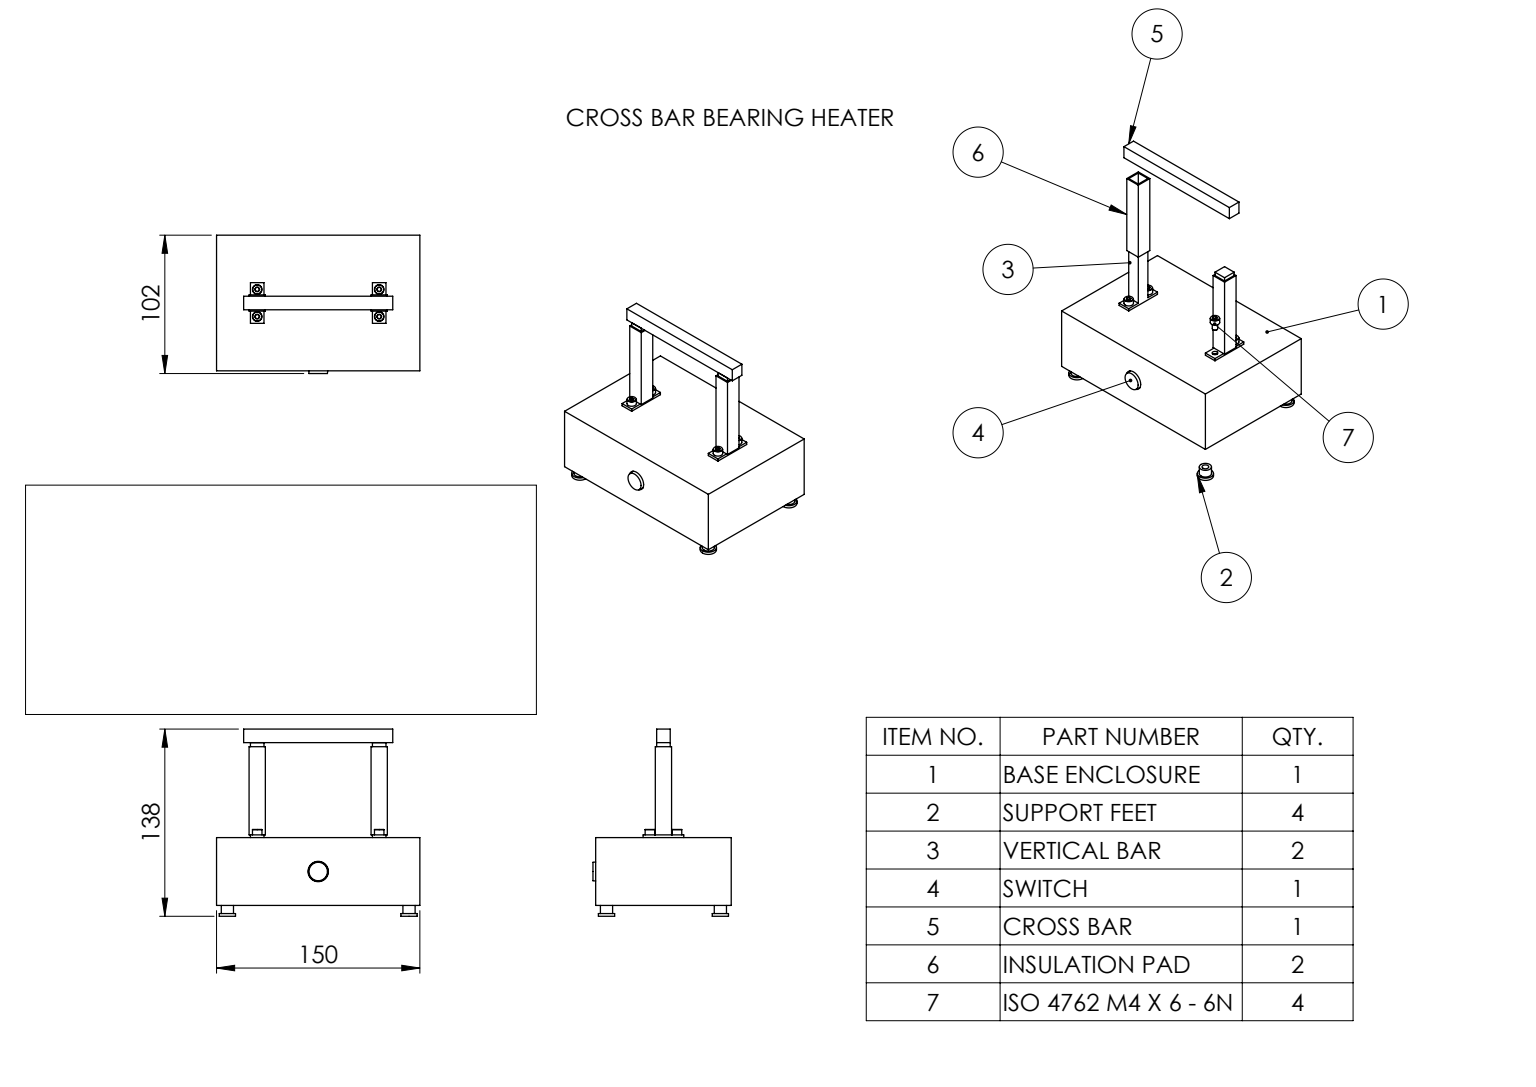
ISO-10303-21;
HEADER;
FILE_DESCRIPTION (('STEP AP214'),
    '1' );
FILE_NAME ('MAS-192',
    '2026-10-24T04:45:50',
    ( '' ),
    ( '' ),
    'SwSTEP 2.0',
    'SolidWorks 2026',
    '' );
FILE_SCHEMA (( 'AUTOMOTIVE_DESIGN' ));
ENDSEC;

DATA;
#1 = ADVANCED_BREP_SHAPE_REPRESENTATION ( '', ( #1992, #3111 ), #2618 ) ;
#2 =( GEOMETRIC_REPRESENTATION_CONTEXT ( 3 ) GLOBAL_UNCERTAINTY_ASSIGNED_CONTEXT ( ( #2528 ) ) GLOBAL_UNIT_ASSIGNED_CONTEXT ( ( #1633, #2133, #1361 ) ) REPRESENTATION_CONTEXT ( 'NONE', 'WORKASPACE' ) );
#3 = DIRECTION ( 'NONE',  ( 0.000000000000000000, -1.000000000000000000, 0.000000000000000000 ) ) ;
#4 = ORIENTED_EDGE ( 'NONE', *, *, #1160, .F. ) ;
#5 = ADVANCED_FACE ( 'NONE', ( #1217, #1180 ), #2474, .T. ) ;
#6 = ORIENTED_EDGE ( 'NONE', *, *, #1808, .T. ) ;
#7 =( GEOMETRIC_REPRESENTATION_CONTEXT ( 3 ) GLOBAL_UNCERTAINTY_ASSIGNED_CONTEXT ( ( #487 ) ) GLOBAL_UNIT_ASSIGNED_CONTEXT ( ( #3000, #1213, #165 ) ) REPRESENTATION_CONTEXT ( 'NONE', 'WORKASPACE' ) );
#8 = DIRECTION ( 'NONE',  ( 0.000000000000000000, 0.000000000000000000, -1.000000000000000000 ) ) ;
#9 = LINE ( 'NONE', #3109, #1942 ) ;
#10 = ORIENTED_EDGE ( 'NONE', *, *, #1397, .T. ) ;
#11 = FACE_OUTER_BOUND ( 'NONE', #1438, .T. ) ;
#12 = FILL_AREA_STYLE_COLOUR ( '', #2947 ) ;
#13 = ORIENTED_EDGE ( 'NONE', *, *, #2082, .F. ) ;
#14 = FACE_OUTER_BOUND ( 'NONE', #3102, .T. ) ;
#15 = FILL_AREA_STYLE_COLOUR ( '', #1949 ) ;
#16 = EDGE_CURVE ( 'NONE', #2394, #756, #2740, .T. ) ;
#17 = DIRECTION ( 'NONE',  ( 0.000000000000000000, 0.000000000000000000, -1.000000000000000000 ) ) ;
#18 = CARTESIAN_POINT ( 'NONE',  ( -49.99999999999999289, 52.00000000000000711, -14.99999999999999645 ) ) ;
#19 = CARTESIAN_POINT ( 'NONE',  ( 66.99999999999997158, -5.000000000000000000, -44.49999999999999289 ) ) ;
#20 = CARTESIAN_POINT ( 'NONE',  ( -40.00000000000000000, 136.9705627484771355, -4.999999999999995559 ) ) ;
#21 = VERTEX_POINT ( 'NONE', #149 ) ;
#22 = VERTEX_POINT ( 'NONE', #1418 ) ;
#23 = CARTESIAN_POINT ( 'NONE',  ( -49.99999999999999289, 136.9705627484771355, -4.999999999999995559 ) ) ;
#24 = EDGE_CURVE ( 'NONE', #3154, #2478, #414, .T. ) ;
#25 = PRODUCT ( 'Support Feet^MAS-192', 'Support Feet^MAS-192', '', ( #945 ) ) ;
#26 = ORIENTED_EDGE ( 'NONE', *, *, #2595, .T. ) ;
#27 = CARTESIAN_POINT ( 'NONE',  ( 2.000000000000000000, -1.773042676681341856, 2.276824562219559311E-15 ) ) ;
#28 = VERTEX_POINT ( 'NONE', #3019 ) ;
#29 = LINE ( 'NONE', #1074, #3100 ) ;
#30 = CARTESIAN_POINT ( 'NONE',  ( -45.00000000000000000, 52.00000000000000711, -7.849999999999996092 ) ) ;
#31 = DIRECTION ( 'NONE',  ( -0.7071067811865355823, 0.000000000000000000, 0.7071067811865595631 ) ) ;
#32 = EDGE_CURVE ( 'NONE', #3203, #1539, #250, .T. ) ;
#33 = LINE ( 'NONE', #1363, #814 ) ;
#34 = ORIENTED_EDGE ( 'NONE', *, *, #997, .F. ) ;
#35 = VERTEX_POINT ( 'NONE', #2248 ) ;
#36 = EDGE_CURVE ( 'NONE', #859, #595, #2266, .T. ) ;
#37 = PLANE ( 'NONE',  #2989 ) ;
#38 = VERTEX_POINT ( 'NONE', #2461 ) ;
#39 = DIRECTION ( 'NONE',  ( -0.000000000000000000, 1.000000000000000000, -0.000000000000000000 ) ) ;
#40 = AXIS2_PLACEMENT_3D ( 'NONE', #1566, #1549, #2083 ) ;
#41 = ORIENTED_EDGE ( 'NONE', *, *, #2652, .T. ) ;
#42 = AXIS2_PLACEMENT_3D ( 'NONE', #131, #167, #900 ) ;
#43 = EDGE_CURVE ( 'NONE', #2320, #2585, #1939, .T. ) ;
#44 = AXIS2_PLACEMENT_3D ( 'NONE', #1214, #1923, #390 ) ;
#45 = LINE ( 'NONE', #1904, #2060 ) ;
#46 =( REPRESENTATION_RELATIONSHIP ('NONE','NONE', #3165, #714 ) REPRESENTATION_RELATIONSHIP_WITH_TRANSFORMATION ( #1813 )SHAPE_REPRESENTATION_RELATIONSHIP( ) );
#47 = AXIS2_PLACEMENT_3D ( 'NONE', #2108, #1339, #2131 ) ;
#48 = FACE_OUTER_BOUND ( 'NONE', #483, .T. ) ;
#49 = AXIS2_PLACEMENT_3D ( 'NONE', #2635, #3135, #2647 ) ;
#50 = CYLINDRICAL_SURFACE ( 'NONE', #2706, 2.000000000000001776 ) ;
#51 = CIRCLE ( 'NONE', #1902, 2.000000000000001776 ) ;
#52 = PRODUCT_DEFINITION_SHAPE ( 'NONE', 'NONE',  #3387 ) ;
#53 = CARTESIAN_POINT ( 'NONE',  ( -51.00000000000000000, 52.00000000000000711, -5.999999999999995559 ) ) ;
#54 = COLOUR_RGB ( '',0.8941176470588234615, 0.8941176470588234615, 0.8941176470588234615 ) ;
#55 = AXIS2_PLACEMENT_3D ( 'NONE', #952, #3052, #3261 ) ;
#56 = ORIENTED_EDGE ( 'NONE', *, *, #736, .T. ) ;
#57 = ORIENTED_EDGE ( 'NONE', *, *, #3226, .F. ) ;
#58 = DIRECTION ( 'NONE',  ( -0.000000000000000000, 1.000000000000000000, -0.000000000000000000 ) ) ;
#59 = VECTOR ( 'NONE', #1910, 1000.000000000000000 ) ;
#60 = EDGE_CURVE ( 'NONE', #1345, #1406, #445, .T. ) ;
#61 = ORIENTED_EDGE ( 'NONE', *, *, #3226, .T. ) ;
#62 = CARTESIAN_POINT ( 'NONE',  ( 75.00000000000000000, 0.000000000000000000, 50.00000000000000000 ) ) ;
#63 = SHAPE_REPRESENTATION_RELATIONSHIP ( 'NONE' , 'NONE' ,  #2804, #1506 ) ;
#64 = EDGE_LOOP ( 'NONE', ( #1744, #977, #3089, #1709 ) ) ;
#65 = CARTESIAN_POINT ( 'NONE',  ( 44.99999999999999289, 50.00000000000000000, -10.00000000000000533 ) ) ;
#66 = PRODUCT_DEFINITION ( 'UNKNOWN', '', #1367, #996 ) ;
#67 = LINE ( 'NONE', #1330, #689 ) ;
#68 = DIRECTION ( 'NONE',  ( -1.000000000000000000, -0.000000000000000000, -0.000000000000000000 ) ) ;
#69 = CARTESIAN_POINT ( 'NONE',  ( -45.00000000000000000, 52.00000000000000711, -9.999999999999994671 ) ) ;
#70 = ORIENTED_EDGE ( 'NONE', *, *, #2599, .T. ) ;
#71 = ORIENTED_EDGE ( 'NONE', *, *, #288, .F. ) ;
#72 = LINE ( 'NONE', #1928, #2609 ) ;
#73 = DIRECTION ( 'NONE',  ( 0.000000000000000000, -0.8660254037844391517, -0.4999999999999991673 ) ) ;
#74 = ORIENTED_EDGE ( 'NONE', *, *, #2863, .T. ) ;
#75 = FACE_OUTER_BOUND ( 'NONE', #670, .T. ) ;
#76 = ADVANCED_FACE ( 'NONE', ( #408 ), #1739, .F. ) ;
#77 = UNCERTAINTY_MEASURE_WITH_UNIT (LENGTH_MEASURE( 1.000000000000000082E-05 ), #1447, 'distance_accuracy_value', 'NONE');
#78 = VERTEX_POINT ( 'NONE', #1445 ) ;
#79 = LINE ( 'NONE', #829, #260 ) ;
#80 = SURFACE_STYLE_USAGE ( .BOTH. , #3231 ) ;
#81 = DIRECTION ( 'NONE',  ( 0.000000000000000000, 0.000000000000000000, -1.000000000000000000 ) ) ;
#82 = LINE ( 'NONE', #1653, #2818 ) ;
#83 = CARTESIAN_POINT ( 'NONE',  ( -51.00000000000000711, 136.9705627484771355, 6.000000000000004441 ) ) ;
#84 = VERTEX_POINT ( 'NONE', #2233 ) ;
#85 = EDGE_LOOP ( 'NONE', ( #3218, #1338, #850, #555, #3293 ) ) ;
#86 = CARTESIAN_POINT ( 'NONE',  ( 4.000000000000000000, 0.000000000000000000, 0.000000000000000000 ) ) ;
#87 = DIRECTION ( 'NONE',  ( 0.000000000000000000, 0.000000000000000000, 1.000000000000000000 ) ) ;
#88 = ORIENTED_EDGE ( 'NONE', *, *, #1626, .T. ) ;
#89 = LINE ( 'NONE', #1159, #2710 ) ;
#90 = EDGE_CURVE ( 'NONE', #872, #1203, #2433, .T. ) ;
#91 = ORIENTED_EDGE ( 'NONE', *, *, #1822, .T. ) ;
#92 = DIRECTION ( 'NONE',  ( 0.000000000000000000, 0.000000000000000000, 1.000000000000000000 ) ) ;
#93 = ADVANCED_FACE ( 'NONE', ( #3005 ), #3282, .F. ) ;
#94 = CIRCLE ( 'NONE', #1191, 2.499999999999995115 ) ;
#95 = CARTESIAN_POINT ( 'NONE',  ( 0.1999999999999987899, 4.286263797015736595E-16, -3.500000000000000000 ) ) ;
#96 = CARTESIAN_POINT ( 'NONE',  ( -74.99999999999998579, 50.00000000000000000, -50.00000000000000000 ) ) ;
#97 = AXIS2_PLACEMENT_3D ( 'NONE', #437, #2770, #128 ) ;
#98 = AXIS2_PLACEMENT_3D ( 'NONE', #3255, #906, #600 ) ;
#99 = DIRECTION ( 'NONE',  ( 0.000000000000000000, -1.000000000000000000, -0.000000000000000000 ) ) ;
#100 = ORIENTED_EDGE ( 'NONE', *, *, #3033, .T. ) ;
#101 = CONICAL_SURFACE ( 'NONE', #2881, 7.250000000000000000, 0.08726646259971666819 ) ;
#102 = EDGE_LOOP ( 'NONE', ( #2901, #2851, #579, #3094 ) ) ;
#103 = FACE_BOUND ( 'NONE', #1561, .T. ) ;
#104 = AXIS2_PLACEMENT_3D ( 'NONE', #3003, #1688, #391 ) ;
#105 = PLANE ( 'NONE',  #1846 ) ;
#106 = EDGE_CURVE ( 'NONE', #871, #1696, #686, .T. ) ;
#107 = SHAPE_REPRESENTATION ( 'cross bar', ( #3111 ), #2618 ) ;
#108 = VERTEX_POINT ( 'NONE', #676 ) ;
#109 =( GEOMETRIC_REPRESENTATION_CONTEXT ( 3 ) GLOBAL_UNCERTAINTY_ASSIGNED_CONTEXT ( ( #1070 ) ) GLOBAL_UNIT_ASSIGNED_CONTEXT ( ( #2231, #2739, #2029 ) ) REPRESENTATION_CONTEXT ( 'NONE', 'WORKASPACE' ) );
#110 = DIRECTION ( 'NONE',  ( -1.000000000000000000, -0.000000000000000000, -0.000000000000000000 ) ) ;
#111 = CARTESIAN_POINT ( 'NONE',  ( 0.000000000000000000, 0.000000000000000000, 0.000000000000000000 ) ) ;
#112 = APPLICATION_CONTEXT ( 'automotive_design' ) ;
#113 = VERTEX_POINT ( 'NONE', #494 ) ;
#114 = AXIS2_PLACEMENT_3D ( 'NONE', #1867, #2907, #1373 ) ;
#115 = CARTESIAN_POINT ( 'NONE',  ( 66.99999999999997158, -5.000000000000000000, -39.50000000000000000 ) ) ;
#116 = DIRECTION ( 'NONE',  ( 4.857225732735056709E-15, 0.000000000000000000, 1.000000000000000000 ) ) ;
#117 = CARTESIAN_POINT ( 'NONE',  ( 9.610000000000013642, 2.449293598294707893E-16, -2.000000000000000888 ) ) ;
#118 = ADVANCED_FACE ( 'NONE', ( #1534 ), #3208, .F. ) ;
#119 = CARTESIAN_POINT ( 'NONE',  ( -74.99999999999998579, 50.00000000000000000, -50.00000000000000000 ) ) ;
#120 = ORIENTED_EDGE ( 'NONE', *, *, #698, .T. ) ;
#121 = VERTEX_POINT ( 'NONE', #1820 ) ;
#122 = FACE_BOUND ( 'NONE', #2327, .T. ) ;
#123 = FACE_OUTER_BOUND ( 'NONE', #1619, .T. ) ;
#124 = ORIENTED_EDGE ( 'NONE', *, *, #674, .T. ) ;
#125 = LINE ( 'NONE', #3241, #2277 ) ;
#126 = PRODUCT_CONTEXT ( 'NONE', #916, 'mechanical' ) ;
#127 = ORIENTED_EDGE ( 'NONE', *, *, #1397, .F. ) ;
#128 = DIRECTION ( 'NONE',  ( 1.000000000000000000, 0.000000000000000000, 0.000000000000000000 ) ) ;
#129 = SURFACE_STYLE_FILL_AREA ( #3049 ) ;
#130 = LINE ( 'NONE', #2502, #3267 ) ;
#131 = CARTESIAN_POINT ( 'NONE',  ( 10.00000000000000000, 1.610000000000000098, 0.000000000000000000 ) ) ;
#132 = CARTESIAN_POINT ( 'NONE',  ( -66.99999999999997158, 0.000000000000000000, -41.99999999999999289 ) ) ;
#133 = EDGE_CURVE ( 'NONE', #3190, #3154, #2535, .T. ) ;
#134 = CARTESIAN_POINT ( 'NONE',  ( 0.000000000000000000, 25.00000000000000000, 50.00000000000000000 ) ) ;
#135 = FACE_OUTER_BOUND ( 'NONE', #3028, .T. ) ;
#136 = CARTESIAN_POINT ( 'NONE',  ( 0.000000000000000000, 117.0000000000000000, 0.000000000000000000 ) ) ;
#137 = EDGE_CURVE ( 'NONE', #1848, #2577, #1400, .T. ) ;
#138 = ORIENTED_EDGE ( 'NONE', *, *, #2911, .T. ) ;
#139 = CARTESIAN_POINT ( 'NONE',  ( 10.00000000000000178, 0.000000000000000000, 0.000000000000000000 ) ) ;
#140 = UNCERTAINTY_MEASURE_WITH_UNIT (LENGTH_MEASURE( 1.000000000000000082E-05 ), #3331, 'distance_accuracy_value', 'NONE');
#141 = CARTESIAN_POINT ( 'NONE',  ( 0.000000000000000000, 0.000000000000000000, 0.000000000000000000 ) ) ;
#142 = ORIENTED_EDGE ( 'NONE', *, *, #43, .F. ) ;
#143 = CARTESIAN_POINT ( 'NONE',  ( -49.99999999999998579, 50.00000000000000000, 15.00000000000000888 ) ) ;
#144 = EDGE_CURVE ( 'NONE', #1979, #3353, #770, .T. ) ;
#145 = DIRECTION ( 'NONE',  ( -0.000000000000000000, 1.000000000000000000, -0.000000000000000000 ) ) ;
#146 = DIRECTION ( 'NONE',  ( 0.000000000000000000, -1.000000000000000000, 0.000000000000000000 ) ) ;
#147 = CIRCLE ( 'NONE', #1023, 2.000000000000000888 ) ;
#148 = DIRECTION ( 'NONE',  ( -0.000000000000000000, 1.000000000000000000, -0.000000000000000000 ) ) ;
#149 = CARTESIAN_POINT ( 'NONE',  ( 4.000000000000001776, 0.000000000000000000, -2.200000000000001066 ) ) ;
#150 = AXIS2_PLACEMENT_3D ( 'NONE', #1095, #3156, #1856 ) ;
#151 = DIRECTION ( 'NONE',  ( 1.000000000000000000, 0.000000000000000000, 0.000000000000000000 ) ) ;
#152 = VECTOR ( 'NONE', #2701, 1000.000000000000000 ) ;
#153 = MECHANICAL_DESIGN_GEOMETRIC_PRESENTATION_REPRESENTATION (  '', ( #3211 ), #1787 ) ;
#154 = VECTOR ( 'NONE', #3115, 1000.000000000000114 ) ;
#155 = ORIENTED_EDGE ( 'NONE', *, *, #2097, .T. ) ;
#156 = DIRECTION ( 'NONE',  ( 1.000000000000000000, 0.000000000000000000, -0.000000000000000000 ) ) ;
#157 = VECTOR ( 'NONE', #2892, 1000.000000000000227 ) ;
#158 = CIRCLE ( 'NONE', #2772, 2.499999999999995115 ) ;
#159 = EDGE_CURVE ( 'NONE', #28, #1965, #1834, .T. ) ;
#160 = DIRECTION ( 'NONE',  ( 0.000000000000000000, 0.000000000000000000, -1.000000000000000000 ) ) ;
#161 = MECHANICAL_DESIGN_GEOMETRIC_PRESENTATION_REPRESENTATION (  '', ( #2503 ), #1797 ) ;
#162 = EDGE_LOOP ( 'NONE', ( #2034, #1285, #2151, #1503 ) ) ;
#163 = DIRECTION ( 'NONE',  ( -1.000000000000000000, -0.000000000000000000, -0.000000000000000000 ) ) ;
#164 = VECTOR ( 'NONE', #3281, 1000.000000000000000 ) ;
#165 =( NAMED_UNIT ( * ) SI_UNIT ( $, .STERADIAN. ) SOLID_ANGLE_UNIT ( ) );
#166 = FACE_OUTER_BOUND ( 'NONE', #3168, .T. ) ;
#167 = DIRECTION ( 'NONE',  ( 1.000000000000000000, 0.000000000000000000, 0.000000000000000000 ) ) ;
#168 = ADVANCED_FACE ( 'NONE', ( #219 ), #472, .F. ) ;
#169 = AXIS2_PLACEMENT_3D ( 'NONE', #1933, #1186, #2975 ) ;
#170 = CARTESIAN_POINT ( 'NONE',  ( -75.00000000000000000, 50.00000000000000000, 50.00000000000000000 ) ) ;
#171 = PLANE ( 'NONE',  #1465 ) ;
#172 = DIRECTION ( 'NONE',  ( 0.000000000000000000, 0.000000000000000000, -1.000000000000000000 ) ) ;
#173 = EDGE_LOOP ( 'NONE', ( #2677, #3008, #1781, #962 ) ) ;
#174 = CARTESIAN_POINT ( 'NONE',  ( -44.99999999999999289, 52.00000000000000711, 10.00000000000000533 ) ) ;
#175 = APPLICATION_PROTOCOL_DEFINITION ( 'draft international standard', 'automotive_design', 1998, #2030 ) ;
#176 = ORIENTED_EDGE ( 'NONE', *, *, #433, .T. ) ;
#177 = ADVANCED_FACE ( 'NONE', ( #782 ), #2573, .F. ) ;
#178 = CARTESIAN_POINT ( 'NONE',  ( 44.99999999999999289, 50.00000000000000000, -12.00000000000000711 ) ) ;
#179 = SHAPE_REPRESENTATION_RELATIONSHIP ( 'NONE' , 'NONE' ,  #1050, #930 ) ;
#180 = ORIENTED_EDGE ( 'NONE', *, *, #1149, .T. ) ;
#181 = EDGE_CURVE ( 'NONE', #2222, #1240, #233, .T. ) ;
#182 = DIRECTION ( 'NONE',  ( 0.000000000000000000, 0.4999999999999989453, -0.8660254037844391517 ) ) ;
#183 = DIRECTION ( 'NONE',  ( -0.000000000000000000, 1.000000000000000000, -0.000000000000000000 ) ) ;
#184 = LINE ( 'NONE', #1230, #2344 ) ;
#185 = DIRECTION ( 'NONE',  ( -0.000000000000000000, 1.000000000000000000, 0.000000000000000000 ) ) ;
#186 = CARTESIAN_POINT ( 'NONE',  ( -66.99999999999997158, -5.000000000000000000, -41.99999999999999289 ) ) ;
#187 = ADVANCED_FACE ( 'NONE', ( #2861 ), #2830, .F. ) ;
#188 = ORIENTED_EDGE ( 'NONE', *, *, #783, .T. ) ;
#189 = DIRECTION ( 'NONE',  ( 0.000000000000000000, 0.000000000000000000, 1.000000000000000000 ) ) ;
#190 = VERTEX_POINT ( 'NONE', #1045 ) ;
#191 = CARTESIAN_POINT ( 'NONE',  ( -45.00000000000000000, 43.79827876194489278, -9.999999999999994671 ) ) ;
#192 = ORIENTED_EDGE ( 'NONE', *, *, #815, .F. ) ;
#193 = DIRECTION ( 'NONE',  ( -4.857225732735056709E-15, 0.000000000000000000, -1.000000000000000000 ) ) ;
#194 = CARTESIAN_POINT ( 'NONE',  ( -49.99999999999999289, 52.00000000000000711, -4.999999999999995559 ) ) ;
#195 = EDGE_CURVE ( 'NONE', #2855, #2405, #2542, .T. ) ;
#196 = CARTESIAN_POINT ( 'NONE',  ( -51.00000000000000000, 136.9705627484771355, -5.999999999999995559 ) ) ;
#197 = DIRECTION ( 'NONE',  ( -0.000000000000000000, 1.000000000000000000, -0.000000000000000000 ) ) ;
#198 = CARTESIAN_POINT ( 'NONE',  ( -50.00000000000000000, 120.0000000000000142, 5.000000000000004441 ) ) ;
#199 = DIRECTION ( 'NONE',  ( 0.000000000000000000, 0.000000000000000000, -1.000000000000000000 ) ) ;
#200 = EDGE_LOOP ( 'NONE', ( #2592, #100, #1336, #1799 ) ) ;
#201 = VECTOR ( 'NONE', #2928, 1000.000000000000000 ) ;
#202 = CIRCLE ( 'NONE', #44, 6.812556682370379590 ) ;
#203 = ORIENTED_EDGE ( 'NONE', *, *, #133, .F. ) ;
#204 = LINE ( 'NONE', #550, #154 ) ;
#205 = EDGE_CURVE ( 'NONE', #575, #3353, #2981, .T. ) ;
#206 = AXIS2_PLACEMENT_3D ( 'NONE', #944, #2253, #978 ) ;
#207 = ITEM_DEFINED_TRANSFORMATION ( 'NONE', 'NONE', #710,  #3111 ) ;
#208 = ORIENTED_EDGE ( 'NONE', *, *, #1510, .T. ) ;
#209 = CIRCLE ( 'NONE', #2120, 2.499999999999995115 ) ;
#210 = CIRCLE ( 'NONE', #2393, 0.2000000000000000944 ) ;
#211 = DIRECTION ( 'NONE',  ( 0.000000000000000000, -1.000000000000000000, 0.000000000000000000 ) ) ;
#212 = AXIS2_PLACEMENT_3D ( 'NONE', #1617, #2642, #885 ) ;
#213 = VECTOR ( 'NONE', #1718, 1000.000000000000000 ) ;
#214 = ORIENTED_EDGE ( 'NONE', *, *, #2529, .F. ) ;
#215 = CARTESIAN_POINT ( 'NONE',  ( -40.00000000000000000, 52.00000000000000711, -4.999999999999995559 ) ) ;
#216 =( NAMED_UNIT ( * ) PLANE_ANGLE_UNIT ( ) SI_UNIT ( $, .RADIAN. ) );
#217 = CARTESIAN_POINT ( 'NONE',  ( -45.00000000000000000, 50.00000000000000000, -9.999999999999994671 ) ) ;
#218 = PRESENTATION_LAYER_ASSIGNMENT (  '', '', ( #384 ) ) ;
#219 = FACE_OUTER_BOUND ( 'NONE', #3264, .T. ) ;
#220 = EDGE_CURVE ( 'NONE', #2968, #788, #147, .T. ) ;
#221 = DIRECTION ( 'NONE',  ( 0.000000000000000000, 0.4999999999999989453, -0.8660254037844391517 ) ) ;
#222 = DIRECTION ( 'NONE',  ( -0.000000000000000000, 1.000000000000000000, -0.000000000000000000 ) ) ;
#223 = VERTEX_POINT ( 'NONE', #2047 ) ;
#224 = ORIENTED_EDGE ( 'NONE', *, *, #1328, .F. ) ;
#225 = FACE_OUTER_BOUND ( 'NONE', #834, .T. ) ;
#226 = ORIENTED_EDGE ( 'NONE', *, *, #721, .T. ) ;
#227 = CARTESIAN_POINT ( 'NONE',  ( 7.500000000000000000, 25.00000000000000000, 50.00000000000000000 ) ) ;
#228 =( NAMED_UNIT ( * ) SI_UNIT ( $, .STERADIAN. ) SOLID_ANGLE_UNIT ( ) );
#229 = VERTEX_POINT ( 'NONE', #2063 ) ;
#230 =( NAMED_UNIT ( * ) SI_UNIT ( $, .STERADIAN. ) SOLID_ANGLE_UNIT ( ) );
#231 = CARTESIAN_POINT ( 'NONE',  ( 2.000000000000000000, 1.773042676681340524, -2.059984127722458425E-15 ) ) ;
#232 = CARTESIAN_POINT ( 'NONE',  ( 45.00000000000000000, 50.00000000000000000, 9.999999999999994671 ) ) ;
#233 = LINE ( 'NONE', #18, #635 ) ;
#234 = CARTESIAN_POINT ( 'NONE',  ( 66.99999999999997158, 0.000000000000000000, -41.99999999999999289 ) ) ;
#235 = PRODUCT ( 'vertical bar^MAS-192', 'vertical bar^MAS-192', '', ( #1405 ) ) ;
#236 = ADVANCED_FACE ( 'NONE', ( #2285 ), #2096, .F. ) ;
#237 = EDGE_LOOP ( 'NONE', ( #1273, #3223, #1162, #2040 ) ) ;
#238 = ORIENTED_EDGE ( 'NONE', *, *, #3134, .T. ) ;
#239 = DIRECTION ( 'NONE',  ( 1.000000000000000000, 0.000000000000000000, 0.000000000000000000 ) ) ;
#240 = PRODUCT_DEFINITION_CONTEXT ( 'detailed design', #1502, 'design' ) ;
#241 = EDGE_CURVE ( 'NONE', #1406, #684, #9, .T. ) ;
#242 = CONTEXT_DEPENDENT_SHAPE_REPRESENTATION ( #1463, #296 ) ;
#243 = EDGE_LOOP ( 'NONE', ( #2805, #1759, #1997, #2614 ) ) ;
#244 = DIRECTION ( 'NONE',  ( 0.000000000000000000, 0.000000000000000000, 1.000000000000000000 ) ) ;
#245 = ORIENTED_EDGE ( 'NONE', *, *, #2920, .T. ) ;
#246 = CARTESIAN_POINT ( 'NONE',  ( -44.99999999999999289, 45.00000000000000711, 12.00000000000000711 ) ) ;
#247 = SURFACE_SIDE_STYLE ('',( #3334 ) ) ;
#248 = EDGE_CURVE ( 'NONE', #1538, #561, #458, .T. ) ;
#249 = CARTESIAN_POINT ( 'NONE',  ( 0.000000000000000000, 0.8865213383406715941, 1.535499999999999199 ) ) ;
#250 = CIRCLE ( 'NONE', #2594, 2.000000000000001776 ) ;
#251 = CARTESIAN_POINT ( 'NONE',  ( -66.99999999999997158, -6.000000000000000000, 41.99999999999999289 ) ) ;
#252 = DIRECTION ( 'NONE',  ( 0.000000000000000000, 0.000000000000000000, 1.000000000000000000 ) ) ;
#253 = CARTESIAN_POINT ( 'NONE',  ( -40.00000000000000000, 52.00000000000000711, 5.000000000000004441 ) ) ;
#254 = ORIENTED_EDGE ( 'NONE', *, *, #2827, .T. ) ;
#255 = ORIENTED_EDGE ( 'NONE', *, *, #1651, .T. ) ;
#256 = PLANE ( 'NONE',  #3270 ) ;
#257 = CIRCLE ( 'NONE', #2169, 0.2000000000000000944 ) ;
#258 = EDGE_LOOP ( 'NONE', ( #2050, #2619 ) ) ;
#259 = EDGE_CURVE ( 'NONE', #2577, #1848, #1348, .T. ) ;
#260 = VECTOR ( 'NONE', #1128, 1000.000000000000000 ) ;
#261 = CARTESIAN_POINT ( 'NONE',  ( -66.99999999999997158, -8.000000000000000000, 41.99999999999999289 ) ) ;
#262 = CIRCLE ( 'NONE', #1350, 1.610000000000000098 ) ;
#263 = AXIS2_PLACEMENT_3D ( 'NONE', #2360, #1555, #2633 ) ;
#264 = ORIENTED_EDGE ( 'NONE', *, *, #1320, .T. ) ;
#265 = DIRECTION ( 'NONE',  ( 0.000000000000000000, 0.000000000000000000, -1.000000000000000000 ) ) ;
#266 = PRODUCT_DEFINITION_SHAPE ( 'NONE', 'NONE',  #2270 ) ;
#267 = DIRECTION ( 'NONE',  ( -0.000000000000000000, -1.000000000000000000, -0.000000000000000000 ) ) ;
#268 = AXIS2_PLACEMENT_3D ( 'NONE', #2067, #1047, #3088 ) ;
#269 = VECTOR ( 'NONE', #221, 1000.000000000000227 ) ;
#270 = CYLINDRICAL_SURFACE ( 'NONE', #435, 2.000000000000001776 ) ;
#271 = VECTOR ( 'NONE', #3335, 1000.000000000000000 ) ;
#272 = DIRECTION ( 'NONE',  ( 1.000000000000000000, 0.000000000000000000, 0.000000000000000000 ) ) ;
#273 = PRODUCT_DEFINITION ( 'UNKNOWN', '', #2401, #2052 ) ;
#274 = CARTESIAN_POINT ( 'NONE',  ( 2.000000000000000000, -1.773042676681341856, 2.276824562219559311E-15 ) ) ;
#275 = PRESENTATION_LAYER_ASSIGNMENT (  '', '', ( #1313 ) ) ;
#276 = CARTESIAN_POINT ( 'NONE',  ( 7.250000000000000000, 25.00000000000000000, 47.00000000000000000 ) ) ;
#277 = VERTEX_POINT ( 'NONE', #2558 ) ;
#278 = ORIENTED_EDGE ( 'NONE', *, *, #1945, .T. ) ;
#279 = AXIS2_PLACEMENT_3D ( 'NONE', #1513, #2605, #2846 ) ;
#280 = DIRECTION ( 'NONE',  ( 0.000000000000000000, 0.000000000000000000, -1.000000000000000000 ) ) ;
#281 = ORIENTED_EDGE ( 'NONE', *, *, #304, .T. ) ;
#282 = DIRECTION ( 'NONE',  ( -1.000000000000000000, 0.000000000000000000, 0.000000000000000000 ) ) ;
#283 = EDGE_CURVE ( 'NONE', #2585, #480, #1268, .T. ) ;
#284 =( NAMED_UNIT ( * ) SI_UNIT ( $, .STERADIAN. ) SOLID_ANGLE_UNIT ( ) );
#285 = ORIENTED_EDGE ( 'NONE', *, *, #1596, .F. ) ;
#286 = CARTESIAN_POINT ( 'NONE',  ( 75.00000000000000000, 50.00000000000000000, 50.00000000000000000 ) ) ;
#287 = APPLICATION_CONTEXT ( 'automotive_design' ) ;
#288 = EDGE_CURVE ( 'NONE', #788, #2968, #3262, .T. ) ;
#289 = FACE_OUTER_BOUND ( 'NONE', #2539, .T. ) ;
#290 = DIRECTION ( 'NONE',  ( -0.000000000000000000, 1.000000000000000000, -0.000000000000000000 ) ) ;
#291 = CYLINDRICAL_SURFACE ( 'NONE', #701, 4.500000000000010658 ) ;
#292 = ORIENTED_EDGE ( 'NONE', *, *, #3182, .F. ) ;
#293 = ORIENTED_EDGE ( 'NONE', *, *, #658, .F. ) ;
#294 = CYLINDRICAL_SURFACE ( 'NONE', #263, 2.000000000000001776 ) ;
#295 = EDGE_CURVE ( 'NONE', #1203, #575, #3205, .T. ) ;
#296 = PRODUCT_DEFINITION_SHAPE ( 'NONE', 'NONE',  #3383 ) ;
#297 = ORIENTED_EDGE ( 'NONE', *, *, #467, .F. ) ;
#298 = CYLINDRICAL_SURFACE ( 'NONE', #3325, 2.499999999999995115 ) ;
#299 = ORIENTED_EDGE ( 'NONE', *, *, #1600, .T. ) ;
#300 = DIRECTION ( 'NONE',  ( -0.000000000000000000, 1.000000000000000000, -0.000000000000000000 ) ) ;
#301 = SURFACE_STYLE_USAGE ( .BOTH. , #1377 ) ;
#302 = FACE_BOUND ( 'NONE', #1880, .T. ) ;
#303 = PLANE ( 'NONE',  #477 ) ;
#304 = EDGE_CURVE ( 'NONE', #820, #28, #1614, .T. ) ;
#305 = LINE ( 'NONE', #901, #2667 ) ;
#306 = ORIENTED_EDGE ( 'NONE', *, *, #1644, .T. ) ;
#307 = ORIENTED_EDGE ( 'NONE', *, *, #2205, .T. ) ;
#308 = LINE ( 'NONE', #1347, #2939 ) ;
#309 = VERTEX_POINT ( 'NONE', #1378 ) ;
#310 = EDGE_CURVE ( 'NONE', #2398, #468, #2110, .T. ) ;
#311 = FACE_OUTER_BOUND ( 'NONE', #2869, .T. ) ;
#312 = CARTESIAN_POINT ( 'NONE',  ( 0.000000000000000000, 0.000000000000000000, 0.000000000000000000 ) ) ;
#313 = ORIENTED_EDGE ( 'NONE', *, *, #934, .T. ) ;
#314 = AXIS2_PLACEMENT_3D ( 'NONE', #1704, #183, #1430 ) ;
#315 = ADVANCED_BREP_SHAPE_REPRESENTATION ( '', ( #2820, #3111 ), #7 ) ;
#316 = LINE ( 'NONE', #2146, #2603 ) ;
#317 = CIRCLE ( 'NONE', #47, 7.250000000000000000 ) ;
#318 = CIRCLE ( 'NONE', #2498, 2.149999999999999023 ) ;
#319 = DIRECTION ( 'NONE',  ( 0.000000000000000000, -1.000000000000000000, 0.000000000000000000 ) ) ;
#320 = AXIS2_PLACEMENT_3D ( 'NONE', #3066, #1000, #486 ) ;
#321 = LINE ( 'NONE', #1331, #636 ) ;
#322 = AXIS2_PLACEMENT_3D ( 'NONE', #1317, #3110, #3142 ) ;
#323 = CARTESIAN_POINT ( 'NONE',  ( 45.00000000000000000, 45.00000000000000711, 7.999999999999992895 ) ) ;
#324 = VECTOR ( 'NONE', #1168, 999.9999999999998863 ) ;
#325 = EDGE_CURVE ( 'NONE', #1539, #3203, #1947, .T. ) ;
#326 = ORIENTED_EDGE ( 'NONE', *, *, #789, .T. ) ;
#327 = EDGE_LOOP ( 'NONE', ( #1272, #3114, #2142, #1931 ) ) ;
#328 = FACE_OUTER_BOUND ( 'NONE', #327, .T. ) ;
#329 = MECHANICAL_DESIGN_GEOMETRIC_PRESENTATION_REPRESENTATION (  '', ( #1259 ), #109 ) ;
#330 = CYLINDRICAL_SURFACE ( 'NONE', #1898, 2.000000000000001776 ) ;
#331 = VERTEX_POINT ( 'NONE', #2651 ) ;
#332 = LINE ( 'NONE', #2410, #1914 ) ;
#333 =( LENGTH_UNIT ( ) NAMED_UNIT ( * ) SI_UNIT ( .MILLI., .METRE. ) );
#334 = SHAPE_REPRESENTATION_RELATIONSHIP ( 'NONE' , 'NONE' ,  #1286, #3149 ) ;
#335 = ORIENTED_EDGE ( 'NONE', *, *, #1134, .T. ) ;
#336 = DIRECTION ( 'NONE',  ( 6.938893903907228378E-16, 0.000000000000000000, 1.000000000000000000 ) ) ;
#337 = FACE_OUTER_BOUND ( 'NONE', #2632, .T. ) ;
#338 = CARTESIAN_POINT ( 'NONE',  ( 2.000000000000000000, 0.8865213383406680414, -1.535500000000000975 ) ) ;
#339 = LINE ( 'NONE', #83, #1798 ) ;
#340 = ORIENTED_EDGE ( 'NONE', *, *, #1808, .F. ) ;
#341 = ORIENTED_EDGE ( 'NONE', *, *, #1510, .F. ) ;
#342 = DIRECTION ( 'NONE',  ( 1.000000000000000000, 0.000000000000000000, 0.000000000000000000 ) ) ;
#343 = EDGE_CURVE ( 'NONE', #2100, #2365, #797, .T. ) ;
#344 = CARTESIAN_POINT ( 'NONE',  ( -49.99999999999999289, 52.00000000000000711, -14.99999999999999645 ) ) ;
#345 = ORIENTED_EDGE ( 'NONE', *, *, #1998, .T. ) ;
#346 = DIRECTION ( 'NONE',  ( -1.000000000000000000, -0.000000000000000000, -0.000000000000000000 ) ) ;
#347 = VERTEX_POINT ( 'NONE', #3209 ) ;
#348 = CARTESIAN_POINT ( 'NONE',  ( -66.99999999999997158, 0.000000000000000000, 46.50000000000000711 ) ) ;
#349 = SURFACE_STYLE_FILL_AREA ( #2686 ) ;
#350 = DIRECTION ( 'NONE',  ( -0.000000000000000000, 1.000000000000000000, -0.000000000000000000 ) ) ;
#351 = DIRECTION ( 'NONE',  ( 0.000000000000000000, 0.000000000000000000, -1.000000000000000000 ) ) ;
#352 = EDGE_CURVE ( 'NONE', #2026, #820, #262, .T. ) ;
#353 = FACE_OUTER_BOUND ( 'NONE', #793, .T. ) ;
#354 = ORIENTED_EDGE ( 'NONE', *, *, #2172, .F. ) ;
#355 = EDGE_LOOP ( 'NONE', ( #2017, #2646, #2374, #1630 ) ) ;
#356 = LINE ( 'NONE', #823, #1685 ) ;
#357 = FACE_BOUND ( 'NONE', #1452, .T. ) ;
#358 = ORIENTED_EDGE ( 'NONE', *, *, #750, .T. ) ;
#359 = CARTESIAN_POINT ( 'NONE',  ( -44.99999999999999289, 50.00000000000000000, 10.00000000000000533 ) ) ;
#360 =( NAMED_UNIT ( * ) PLANE_ANGLE_UNIT ( ) SI_UNIT ( $, .RADIAN. ) );
#361 = VERTEX_POINT ( 'NONE', #3180 ) ;
#362 = ADVANCED_FACE ( 'NONE', ( #830 ), #478, .F. ) ;
#363 = LINE ( 'NONE', #1728, #583 ) ;
#364 =( LENGTH_UNIT ( ) NAMED_UNIT ( * ) SI_UNIT ( .MILLI., .METRE. ) );
#365 = MECHANICAL_DESIGN_GEOMETRIC_PRESENTATION_REPRESENTATION (  '', ( #2220 ), #1676 ) ;
#366 = AXIS2_PLACEMENT_3D ( 'NONE', #1458, #3294, #1985 ) ;
#367 = FACE_OUTER_BOUND ( 'NONE', #3150, .T. ) ;
#368 = DIRECTION ( 'NONE',  ( 0.000000000000000000, 0.000000000000000000, 1.000000000000000000 ) ) ;
#369 = VECTOR ( 'NONE', #2367, 1000.000000000000000 ) ;
#370 = CIRCLE ( 'NONE', #482, 4.500000000000010658 ) ;
#371 = DIRECTION ( 'NONE',  ( -1.000000000000000000, -0.000000000000000000, -0.000000000000000000 ) ) ;
#372 = ORIENTED_EDGE ( 'NONE', *, *, #3079, .F. ) ;
#373 = AXIS2_PLACEMENT_3D ( 'NONE', #3007, #3300, #957 ) ;
#374 = EDGE_CURVE ( 'NONE', #2968, #21, #257, .T. ) ;
#375 = CIRCLE ( 'NONE', #1306, 2.499999999999995115 ) ;
#376 = ORIENTED_EDGE ( 'NONE', *, *, #1556, .T. ) ;
#377 = FACE_BOUND ( 'NONE', #2636, .T. ) ;
#378 = CIRCLE ( 'NONE', #212, 3.500000000000000000 ) ;
#379 = AXIS2_PLACEMENT_3D ( 'NONE', #915, #146, #2518 ) ;
#380 = DIRECTION ( 'NONE',  ( 0.000000000000000000, -0.000000000000000000, 1.000000000000000000 ) ) ;
#381 = ORIENTED_EDGE ( 'NONE', *, *, #248, .F. ) ;
#382 = CIRCLE ( 'NONE', #279, 2.499999999999995115 ) ;
#383 = CARTESIAN_POINT ( 'NONE',  ( 2.000000000000000000, 0.000000000000000000, 0.000000000000000000 ) ) ;
#384 = STYLED_ITEM ( 'NONE', ( #3081 ), #1 ) ;
#385 = DIRECTION ( 'NONE',  ( 0.000000000000000000, 0.000000000000000000, -1.000000000000000000 ) ) ;
#386 = ORIENTED_EDGE ( 'NONE', *, *, #1705, .F. ) ;
#387 = AXIS2_PLACEMENT_3D ( 'NONE', #2488, #151, #2249 ) ;
#388 = DIRECTION ( 'NONE',  ( 0.000000000000000000, 0.000000000000000000, -1.000000000000000000 ) ) ;
#389 = ADVANCED_FACE ( 'NONE', ( #337 ), #751, .T. ) ;
#390 = DIRECTION ( 'NONE',  ( 1.000000000000000000, 0.000000000000000000, 0.000000000000000000 ) ) ;
#391 = DIRECTION ( 'NONE',  ( 0.000000000000000000, 1.224646799147353207E-16, 1.000000000000000000 ) ) ;
#392 = EDGE_CURVE ( 'NONE', #2543, #2273, #1858, .T. ) ;
#393 = FACE_OUTER_BOUND ( 'NONE', #821, .T. ) ;
#394 = DIRECTION ( 'NONE',  ( 0.000000000000000000, 0.000000000000000000, 1.000000000000000000 ) ) ;
#395 = CARTESIAN_POINT ( 'NONE',  ( 2.000000000000000000, -0.8865213383406694847, 1.535500000000001419 ) ) ;
#396 = APPLICATION_CONTEXT ( 'automotive_design' ) ;
#397 = DIRECTION ( 'NONE',  ( 0.000000000000000000, 0.4999999999999991118, -0.8660254037844390407 ) ) ;
#398 = ORIENTED_EDGE ( 'NONE', *, *, #2812, .T. ) ;
#399 = DIRECTION ( 'NONE',  ( -0.000000000000000000, 1.000000000000000000, -0.000000000000000000 ) ) ;
#400 = ADVANCED_FACE ( 'NONE', ( #302, #1340 ), #2369, .F. ) ;
#401 = PRODUCT_CONTEXT ( 'NONE', #1167, 'mechanical' ) ;
#402 = ORIENTED_EDGE ( 'NONE', *, *, #3206, .F. ) ;
#403 = CARTESIAN_POINT ( 'NONE',  ( 66.99999999999997158, -5.000000000000000000, -41.99999999999999289 ) ) ;
#404 = FILL_AREA_STYLE_COLOUR ( '', #874 ) ;
#405 = CARTESIAN_POINT ( 'NONE',  ( -66.99999999999997158, -8.000000000000000000, 39.49999999999998579 ) ) ;
#406 = CARTESIAN_POINT ( 'NONE',  ( -51.00000000000000000, 136.9705627484771355, -4.999999999999996447 ) ) ;
#407 = CARTESIAN_POINT ( 'NONE',  ( -45.00000000000000000, 50.00000000000000000, -7.999999999999992895 ) ) ;
#408 = FACE_OUTER_BOUND ( 'NONE', #1187, .T. ) ;
#409 = EDGE_CURVE ( 'NONE', #2129, #108, #67, .T. ) ;
#410 = DIRECTION ( 'NONE',  ( -1.000000000000000000, -0.000000000000000000, 2.365532012695647326E-17 ) ) ;
#411 = ORIENTED_EDGE ( 'NONE', *, *, #2806, .T. ) ;
#412 = PLANE ( 'NONE',  #1407 ) ;
#413 = DIRECTION ( 'NONE',  ( -1.000000000000000000, 0.000000000000000000, 0.000000000000000000 ) ) ;
#414 = CIRCLE ( 'NONE', #849, 7.500000000000000000 ) ;
#415 = ORIENTED_EDGE ( 'NONE', *, *, #2685, .T. ) ;
#416 = EDGE_CURVE ( 'NONE', #2252, #436, #1895, .T. ) ;
#417 = CARTESIAN_POINT ( 'NONE',  ( 55.00000000000000000, 130.0000000000000000, -5.000000000000000000 ) ) ;
#418 = LINE ( 'NONE', #2471, #152 ) ;
#419 = CARTESIAN_POINT ( 'NONE',  ( -50.00000000000000000, 117.0000000000000000, 5.000000000000004441 ) ) ;
#420 = DIRECTION ( 'NONE',  ( 0.000000000000000000, -1.000000000000000000, 0.000000000000000000 ) ) ;
#421 = CARTESIAN_POINT ( 'NONE',  ( -45.00000000000000000, 50.00000000000000000, -9.999999999999994671 ) ) ;
#422 = CIRCLE ( 'NONE', #2330, 2.500000000000009326 ) ;
#423 = DIRECTION ( 'NONE',  ( 0.000000000000000000, -1.000000000000000000, 0.000000000000000000 ) ) ;
#424 = AXIS2_PLACEMENT_3D ( 'NONE', #2897, #2673, #1362 ) ;
#425 = ADVANCED_FACE ( 'NONE', ( #48 ), #847, .T. ) ;
#426 =( NAMED_UNIT ( * ) SI_UNIT ( $, .STERADIAN. ) SOLID_ANGLE_UNIT ( ) );
#427 = AXIS2_PLACEMENT_3D ( 'NONE', #2477, #1108, #87 ) ;
#428 = AXIS2_PLACEMENT_3D ( 'NONE', #139, #1256, #3320 ) ;
#429 = ORIENTED_EDGE ( 'NONE', *, *, #1320, .F. ) ;
#430 = LINE ( 'NONE', #1761, #2389 ) ;
#431 = AXIS2_PLACEMENT_3D ( 'NONE', #2899, #2590, #546 ) ;
#432 = VECTOR ( 'NONE', #2012, 999.9999999999998863 ) ;
#433 = EDGE_CURVE ( 'NONE', #2761, #2259, #1907, .T. ) ;
#434 = DIRECTION ( 'NONE',  ( 1.000000000000000000, 0.000000000000000000, 0.000000000000000000 ) ) ;
#435 = AXIS2_PLACEMENT_3D ( 'NONE', #232, #1280, #3107 ) ;
#436 = VERTEX_POINT ( 'NONE', #95 ) ;
#437 = CARTESIAN_POINT ( 'NONE',  ( 0.000000000000000000, 25.00000000000000000, 47.00000000000000000 ) ) ;
#438 = STYLED_ITEM ( 'NONE', ( #1597 ), #3149 ) ;
#439 =( NAMED_UNIT ( * ) PLANE_ANGLE_UNIT ( ) SI_UNIT ( $, .RADIAN. ) );
#440 = ORIENTED_EDGE ( 'NONE', *, *, #90, .F. ) ;
#441 = CARTESIAN_POINT ( 'NONE',  ( 55.00000000000004974, 130.0000000000000000, 5.000000000000004441 ) ) ;
#442 = PLANE ( 'NONE',  #2112 ) ;
#443 = EDGE_CURVE ( 'NONE', #277, #2259, #3036, .T. ) ;
#444 = DIRECTION ( 'NONE',  ( -0.000000000000000000, 1.000000000000000000, -0.000000000000000000 ) ) ;
#445 = LINE ( 'NONE', #3298, #1076 ) ;
#446 = DIRECTION ( 'NONE',  ( -0.000000000000000000, 0.8660254037844392627, 0.4999999999999990008 ) ) ;
#447 =( LENGTH_UNIT ( ) NAMED_UNIT ( * ) SI_UNIT ( .MILLI., .METRE. ) );
#448 = VERTEX_POINT ( 'NONE', #2198 ) ;
#449 = LINE ( 'NONE', #959, #1301 ) ;
#450 = CONTEXT_DEPENDENT_SHAPE_REPRESENTATION ( #2246, #946 ) ;
#451 = EDGE_LOOP ( 'NONE', ( #1435, #993, #1013, #2138 ) ) ;
#452 = ADVANCED_FACE ( 'NONE', ( #1953 ), #2723, .F. ) ;
#453 = PLANE ( 'NONE',  #2663 ) ;
#454 = ORIENTED_EDGE ( 'NONE', *, *, #1869, .T. ) ;
#455 = PRODUCT ( 'MAS-192', 'MAS-192', '', ( #659 ) ) ;
#456 = SURFACE_STYLE_USAGE ( .BOTH. , #2352 ) ;
#457 = CARTESIAN_POINT ( 'NONE',  ( -54.99999999999995026, 120.0000000000000142, 5.000000000000004441 ) ) ;
#458 = LINE ( 'NONE', #1514, #910 ) ;
#459 = EDGE_CURVE ( 'NONE', #756, #1406, #418, .T. ) ;
#460 = LINE ( 'NONE', #3299, #3221 ) ;
#461 = ORIENTED_EDGE ( 'NONE', *, *, #1991, .F. ) ;
#462 = ORIENTED_EDGE ( 'NONE', *, *, #144, .F. ) ;
#463 = CARTESIAN_POINT ( 'NONE',  ( -66.99999999999997158, -5.000000000000000000, 39.50000000000000000 ) ) ;
#464 = CONTEXT_DEPENDENT_SHAPE_REPRESENTATION ( #565, #2882 ) ;
#465 = ORIENTED_EDGE ( 'NONE', *, *, #2720, .F. ) ;
#466 = PLANE ( 'NONE',  #320 ) ;
#467 = EDGE_CURVE ( 'NONE', #2054, #940, #3232, .T. ) ;
#468 = VERTEX_POINT ( 'NONE', #1178 ) ;
#469 = SURFACE_STYLE_USAGE ( .BOTH. , #2602 ) ;
#470 = DIRECTION ( 'NONE',  ( 1.049727191138620668E-16, 0.5150380749100514910, -0.8571673007021138879 ) ) ;
#471 = DIRECTION ( 'NONE',  ( -0.000000000000000000, 1.000000000000000000, -0.000000000000000000 ) ) ;
#472 = CYLINDRICAL_SURFACE ( 'NONE', #803, 2.500000000000009326 ) ;
#473 = CARTESIAN_POINT ( 'NONE',  ( -45.00000000000000000, 50.00000000000000000, -9.999999999999994671 ) ) ;
#474 = AXIS2_PLACEMENT_3D ( 'NONE', #3365, #715, #2588 ) ;
#475 = DIRECTION ( 'NONE',  ( 0.000000000000000000, -1.000000000000000000, 0.000000000000000000 ) ) ;
#476 = ORIENTED_EDGE ( 'NONE', *, *, #2240, .T. ) ;
#477 = AXIS2_PLACEMENT_3D ( 'NONE', #2403, #3181, #1342 ) ;
#478 = CONICAL_SURFACE ( 'NONE', #424, 2.000000000000001776, 1.029744258676657642 ) ;
#479 = ADVANCED_BREP_SHAPE_REPRESENTATION ( '', ( #2792, #3111 ), #1204 ) ;
#480 = VERTEX_POINT ( 'NONE', #2212 ) ;
#481 = DIRECTION ( 'NONE',  ( 0.000000000000000000, -0.000000000000000000, -1.000000000000000000 ) ) ;
#482 = AXIS2_PLACEMENT_3D ( 'NONE', #711, #2825, #1752 ) ;
#483 = EDGE_LOOP ( 'NONE', ( #402, #2152, #70, #1488 ) ) ;
#484 = CIRCLE ( 'NONE', #975, 6.000000000000005329 ) ;
#485 = VECTOR ( 'NONE', #1029, 1000.000000000000000 ) ;
#486 = DIRECTION ( 'NONE',  ( 0.000000000000000000, -0.000000000000000000, -1.000000000000000000 ) ) ;
#487 = UNCERTAINTY_MEASURE_WITH_UNIT (LENGTH_MEASURE( 1.000000000000000082E-05 ), #3000, 'distance_accuracy_value', 'NONE');
#488 = VECTOR ( 'NONE', #2883, 1000.000000000000000 ) ;
#489 = VERTEX_POINT ( 'NONE', #1686 ) ;
#490 = CARTESIAN_POINT ( 'NONE',  ( -39.00000000000000000, 52.00000000000000711, -5.999999999999995559 ) ) ;
#491 = DIRECTION ( 'NONE',  ( -0.000000000000000000, -1.000000000000000000, -0.000000000000000000 ) ) ;
#492 = ADVANCED_FACE ( 'NONE', ( #3247 ), #1936, .F. ) ;
#493 = LINE ( 'NONE', #2046, #2452 ) ;
#494 = CARTESIAN_POINT ( 'NONE',  ( 44.99999999999999289, 45.00000000000000711, -8.000000000000003553 ) ) ;
#495 = CARTESIAN_POINT ( 'NONE',  ( 75.00000000000000000, 0.000000000000000000, -50.00000000000000000 ) ) ;
#496 = EDGE_CURVE ( 'NONE', #1994, #2222, #130, .T. ) ;
#497 = AXIS2_PLACEMENT_3D ( 'NONE', #554, #1610, #2648 ) ;
#498 = ORIENTED_EDGE ( 'NONE', *, *, #1764, .F. ) ;
#499 = VERTEX_POINT ( 'NONE', #1703 ) ;
#500 = LINE ( 'NONE', #2579, #1737 ) ;
#501 = ITEM_DEFINED_TRANSFORMATION ( 'NONE', 'NONE', #2347,  #3111 ) ;
#502 = ORIENTED_EDGE ( 'NONE', *, *, #2853, .F. ) ;
#503 = EDGE_CURVE ( 'NONE', #2959, #3196, #202, .T. ) ;
#504 = DIRECTION ( 'NONE',  ( 0.000000000000000000, 0.000000000000000000, 1.000000000000000000 ) ) ;
#505 = SURFACE_SIDE_STYLE ('',( #2583 ) ) ;
#506 = EDGE_LOOP ( 'NONE', ( #2297, #1009 ) ) ;
#507 = FACE_OUTER_BOUND ( 'NONE', #752, .T. ) ;
#508 = CARTESIAN_POINT ( 'NONE',  ( -66.99999999999997158, -8.000000000000000000, 41.99999999999999289 ) ) ;
#509 = LINE ( 'NONE', #2809, #1520 ) ;
#510 = PRODUCT ( 'Base Enclosure^MAS-192', 'Base Enclosure^MAS-192', '', ( #126 ) ) ;
#511 = EDGE_CURVE ( 'NONE', #1605, #1554, #94, .T. ) ;
#512 = ORIENTED_EDGE ( 'NONE', *, *, #2624, .F. ) ;
#513 = EDGE_LOOP ( 'NONE', ( #1170, #1121 ) ) ;
#514 = PLANE ( 'NONE',  #2007 ) ;
#515 = EDGE_LOOP ( 'NONE', ( #3254, #1310, #3355, #3169 ) ) ;
#516 = ADVANCED_BREP_SHAPE_REPRESENTATION ( '', ( #3171, #3111 ), #2779 ) ;
#517 = DIRECTION ( 'NONE',  ( -0.000000000000000000, 1.000000000000000000, -0.000000000000000000 ) ) ;
#518 = ADVANCED_FACE ( 'NONE', ( #2751 ), #3260, .T. ) ;
#519 = ORIENTED_EDGE ( 'NONE', *, *, #1564, .F. ) ;
#520 = DIRECTION ( 'NONE',  ( -0.000000000000000000, 1.000000000000000000, -0.000000000000000000 ) ) ;
#521 = CARTESIAN_POINT ( 'NONE',  ( 0.000000000000000000, 120.0000000000000142, 0.000000000000000000 ) ) ;
#522 = DIRECTION ( 'NONE',  ( 0.000000000000000000, -0.5000000000000011102, -0.8660254037844379305 ) ) ;
#523 = LINE ( 'NONE', #2574, #1629 ) ;
#524 =( NAMED_UNIT ( * ) SI_UNIT ( $, .STERADIAN. ) SOLID_ANGLE_UNIT ( ) );
#525 = ORIENTED_EDGE ( 'NONE', *, *, #1492, .F. ) ;
#526 = ORIENTED_EDGE ( 'NONE', *, *, #934, .F. ) ;
#527 = DIRECTION ( 'NONE',  ( -1.000000000000000000, -0.000000000000000000, -0.000000000000000000 ) ) ;
#528 = ADVANCED_FACE ( 'NONE', ( #914 ), #2517, .T. ) ;
#529 = VECTOR ( 'NONE', #491, 1000.000000000000000 ) ;
#530 = COLOUR_RGB ( '',1.000000000000000000, 0.9490196078431372140, 0.9098039215686274384 ) ;
#531 = VERTEX_POINT ( 'NONE', #2484 ) ;
#532 = AXIS2_PLACEMENT_3D ( 'NONE', #403, #2962, #671 ) ;
#533 = CARTESIAN_POINT ( 'NONE',  ( 0.000000000000000000, 0.8865213383406680414, -1.535500000000000975 ) ) ;
#534 = VECTOR ( 'NONE', #1624, 1000.000000000000000 ) ;
#535 = EDGE_CURVE ( 'NONE', #871, #3340, #2736, .T. ) ;
#536 = AXIS2_PLACEMENT_3D ( 'NONE', #3344, #1291, #2041 ) ;
#537 = CIRCLE ( 'NONE', #3045, 2.000000000000001776 ) ;
#538 = ORIENTED_EDGE ( 'NONE', *, *, #496, .F. ) ;
#539 = DIRECTION ( 'NONE',  ( 0.000000000000000000, -1.000000000000000000, 0.000000000000000000 ) ) ;
#540 = VECTOR ( 'NONE', #639, 1000.000000000000000 ) ;
#541 = PLANE ( 'NONE',  #2013 ) ;
#542 = AXIS2_PLACEMENT_3D ( 'NONE', #1565, #1586, #1044 ) ;
#543 = CARTESIAN_POINT ( 'NONE',  ( 2.000000000000000000, 0.8865213383406680414, -1.535500000000000975 ) ) ;
#544 = DIRECTION ( 'NONE',  ( -1.000000000000000000, -0.000000000000000000, -0.000000000000000000 ) ) ;
#545 = EDGE_CURVE ( 'NONE', #28, #788, #2244, .T. ) ;
#546 = DIRECTION ( 'NONE',  ( 0.000000000000000000, 0.000000000000000000, 1.000000000000000000 ) ) ;
#547 = ORIENTED_EDGE ( 'NONE', *, *, #1705, .T. ) ;
#548 = ORIENTED_EDGE ( 'NONE', *, *, #3058, .T. ) ;
#549 = AXIS2_PLACEMENT_3D ( 'NONE', #141, #3041, #1451 ) ;
#550 = CARTESIAN_POINT ( 'NONE',  ( 10.00000000000000178, 1.971681346627238735E-16, -1.610000000000000098 ) ) ;
#551 = ORIENTED_EDGE ( 'NONE', *, *, #1747, .F. ) ;
#552 = DIRECTION ( 'NONE',  ( 0.000000000000000000, 0.000000000000000000, 1.000000000000000000 ) ) ;
#553 = UNCERTAINTY_MEASURE_WITH_UNIT (LENGTH_MEASURE( 1.000000000000000082E-05 ), #1906, 'distance_accuracy_value', 'NONE');
#554 = CARTESIAN_POINT ( 'NONE',  ( 0.000000000000000000, 0.000000000000000000, 0.000000000000000000 ) ) ;
#555 = ORIENTED_EDGE ( 'NONE', *, *, #2172, .T. ) ;
#556 = ADVANCED_FACE ( 'NONE', ( #3015, #1192 ), #2228, .T. ) ;
#557 = CARTESIAN_POINT ( 'NONE',  ( 45.00000000000000000, 45.00000000000000711, 9.999999999999994671 ) ) ;
#558 = DIRECTION ( 'NONE',  ( -1.000000000000000000, 0.000000000000000000, 6.938893903907232322E-16 ) ) ;
#559 = CARTESIAN_POINT ( 'NONE',  ( 0.000000000000000000, 130.0000000000000000, 0.000000000000000000 ) ) ;
#560 = DIRECTION ( 'NONE',  ( 0.08715574274765836016, 0.000000000000000000, -0.9961946980917455452 ) ) ;
#561 = VERTEX_POINT ( 'NONE', #1479 ) ;
#562 = ORIENTED_EDGE ( 'NONE', *, *, #1667, .F. ) ;
#563 = DIRECTION ( 'NONE',  ( -1.000000000000000000, -0.000000000000000000, -0.000000000000000000 ) ) ;
#564 = ORIENTED_EDGE ( 'NONE', *, *, #2324, .F. ) ;
#565 =( REPRESENTATION_RELATIONSHIP ('NONE','NONE', #3165, #936 ) REPRESENTATION_RELATIONSHIP_WITH_TRANSFORMATION ( #1527 )SHAPE_REPRESENTATION_RELATIONSHIP( ) );
#566 = CARTESIAN_POINT ( 'NONE',  ( 0.000000000000000000, 1.773042676681340524, -2.059984127722458425E-15 ) ) ;
#567 =( LENGTH_UNIT ( ) NAMED_UNIT ( * ) SI_UNIT ( .MILLI., .METRE. ) );
#568 = ORIENTED_EDGE ( 'NONE', *, *, #3327, .T. ) ;
#569 = DIRECTION ( 'NONE',  ( -0.000000000000000000, 1.000000000000000000, -0.000000000000000000 ) ) ;
#570 = ADVANCED_FACE ( 'NONE', ( #166 ), #1717, .T. ) ;
#571 = DIRECTION ( 'NONE',  ( 1.000000000000000000, 0.000000000000000000, 0.000000000000000000 ) ) ;
#572 = FACE_OUTER_BOUND ( 'NONE', #3302, .T. ) ;
#573 = MANIFOLD_SOLID_BREP ( 'Hex', #3148 ) ;
#574 = DIRECTION ( 'NONE',  ( 0.000000000000000000, 0.000000000000000000, 1.000000000000000000 ) ) ;
#575 = VERTEX_POINT ( 'NONE', #1278 ) ;
#576 = ORIENTED_EDGE ( 'NONE', *, *, #343, .T. ) ;
#577 = FACE_OUTER_BOUND ( 'NONE', #3185, .T. ) ;
#578 = PLANE ( 'NONE',  #2006 ) ;
#579 = ORIENTED_EDGE ( 'NONE', *, *, #3144, .T. ) ;
#580 = CARTESIAN_POINT ( 'NONE',  ( -45.00000000000000000, 50.00000000000000000, -7.849999999999996092 ) ) ;
#581 = UNCERTAINTY_MEASURE_WITH_UNIT (LENGTH_MEASURE( 1.000000000000000082E-05 ), #795, 'distance_accuracy_value', 'NONE');
#582 = ORIENTED_EDGE ( 'NONE', *, *, #2378, .T. ) ;
#583 = VECTOR ( 'NONE', #2735, 1000.000000000000114 ) ;
#584 = AXIS2_PLACEMENT_3D ( 'NONE', #1266, #520, #989 ) ;
#585 = CARTESIAN_POINT ( 'NONE',  ( -44.99999999999999289, 50.00000000000000000, 10.00000000000000533 ) ) ;
#586 = AXIS2_PLACEMENT_3D ( 'NONE', #2582, #2295, #1015 ) ;
#587 = DIRECTION ( 'NONE',  ( 0.000000000000000000, 0.000000000000000000, 1.000000000000000000 ) ) ;
#588 = ADVANCED_FACE ( 'NONE', ( #367 ), #2004, .F. ) ;
#589 = CIRCLE ( 'NONE', #1031, 4.500000000000010658 ) ;
#590 = DIRECTION ( 'NONE',  ( 0.000000000000000000, 0.000000000000000000, 1.000000000000000000 ) ) ;
#591 = AXIS2_PLACEMENT_3D ( 'NONE', #86, #1136, #2168 ) ;
#592 = DIRECTION ( 'NONE',  ( -1.000000000000000000, -0.000000000000000000, -0.000000000000000000 ) ) ;
#593 = CIRCLE ( 'NONE', #268, 6.000000000000005329 ) ;
#594 = VERTEX_POINT ( 'NONE', #2044 ) ;
#595 = VERTEX_POINT ( 'NONE', #1562 ) ;
#596 = ADVANCED_FACE ( 'NONE', ( #3051 ), #1293, .T. ) ;
#597 = CARTESIAN_POINT ( 'NONE',  ( -44.99999999999999289, 45.00000000000000711, 10.00000000000000533 ) ) ;
#598 = DIRECTION ( 'NONE',  ( 1.000000000000000000, -0.000000000000000000, 1.387778780781445676E-16 ) ) ;
#599 = ORIENTED_EDGE ( 'NONE', *, *, #2055, .T. ) ;
#600 = DIRECTION ( 'NONE',  ( 0.000000000000000000, 0.000000000000000000, -1.000000000000000000 ) ) ;
#601 = FILL_AREA_STYLE_COLOUR ( '', #3001 ) ;
#602 = EDGE_LOOP ( 'NONE', ( #1760, #2359 ) ) ;
#603 = EDGE_CURVE ( 'NONE', #448, #2691, #764, .T. ) ;
#604 = CARTESIAN_POINT ( 'NONE',  ( 2.000000000000000000, 0.8865213383406680414, -1.535500000000000975 ) ) ;
#605 = CARTESIAN_POINT ( 'NONE',  ( 2.000000000000000000, 0.000000000000000000, 0.000000000000000000 ) ) ;
#606 = CARTESIAN_POINT ( 'NONE',  ( -66.99999999999997158, -6.000000000000000000, 44.50000000000000711 ) ) ;
#607 = CARTESIAN_POINT ( 'NONE',  ( 2.000000000000000000, -1.773042676681341856, 2.276824562219559311E-15 ) ) ;
#608 = VERTEX_POINT ( 'NONE', #2329 ) ;
#609 = ORIENTED_EDGE ( 'NONE', *, *, #721, .F. ) ;
#610 = DIRECTION ( 'NONE',  ( 6.938893903907228378E-16, 0.000000000000000000, -1.000000000000000000 ) ) ;
#611 = EDGE_CURVE ( 'NONE', #2086, #347, #1767, .T. ) ;
#612 = DIRECTION ( 'NONE',  ( 0.000000000000000000, 0.000000000000000000, 1.000000000000000000 ) ) ;
#613 = ORIENTED_EDGE ( 'NONE', *, *, #2891, .T. ) ;
#614 = PLANE ( 'NONE',  #3101 ) ;
#615 = UNCERTAINTY_MEASURE_WITH_UNIT (LENGTH_MEASURE( 1.000000000000000082E-05 ), #1164, 'distance_accuracy_value', 'NONE');
#616 = CARTESIAN_POINT ( 'NONE',  ( 0.000000000000000000, 0.000000000000000000, 0.000000000000000000 ) ) ;
#617 = VERTEX_POINT ( 'NONE', #1508 ) ;
#618 = CARTESIAN_POINT ( 'NONE',  ( -45.00000000000000000, 50.00000000000000000, -11.99999999999999645 ) ) ;
#619 = EDGE_CURVE ( 'NONE', #1240, #2273, #742, .T. ) ;
#620 = PRESENTATION_STYLE_ASSIGNMENT (( #301 ) ) ;
#621 = DIRECTION ( 'NONE',  ( 0.000000000000000000, 0.000000000000000000, 1.000000000000000000 ) ) ;
#622 = DIRECTION ( 'NONE',  ( -1.000000000000000000, -0.000000000000000000, -0.000000000000000000 ) ) ;
#623 = FACE_OUTER_BOUND ( 'NONE', #2591, .T. ) ;
#624 = VERTEX_POINT ( 'NONE', #2550 ) ;
#625 = VERTEX_POINT ( 'NONE', #215 ) ;
#626 = DIRECTION ( 'NONE',  ( -0.000000000000000000, 1.000000000000000000, -0.000000000000000000 ) ) ;
#627 = CARTESIAN_POINT ( 'NONE',  ( -40.00000000000000000, 136.9705627484771355, -5.999999999999995559 ) ) ;
#628 = ORIENTED_EDGE ( 'NONE', *, *, #2891, .F. ) ;
#629 = LINE ( 'NONE', #2695, #2935 ) ;
#630 = EDGE_CURVE ( 'NONE', #347, #2291, #3348, .T. ) ;
#631 =( NAMED_UNIT ( * ) SI_UNIT ( $, .STERADIAN. ) SOLID_ANGLE_UNIT ( ) );
#632 = ORIENTED_EDGE ( 'NONE', *, *, #2958, .F. ) ;
#633 = ADVANCED_FACE ( 'NONE', ( #781 ), #2027, .F. ) ;
#634 = LINE ( 'NONE', #948, #2276 ) ;
#635 = VECTOR ( 'NONE', #1006, 1000.000000000000000 ) ;
#636 = VECTOR ( 'NONE', #2965, 1000.000000000000000 ) ;
#637 = AXIS2_PLACEMENT_3D ( 'NONE', #2080, #3362, #966 ) ;
#638 = CARTESIAN_POINT ( 'NONE',  ( 0.000000000000000000, 25.00000000000000000, 52.00000000000000000 ) ) ;
#639 = DIRECTION ( 'NONE',  ( 1.000000000000000000, 0.000000000000000000, 0.000000000000000000 ) ) ;
#640 = CIRCLE ( 'NONE', #1461, 1.610000000000000098 ) ;
#641 = AXIS2_PLACEMENT_3D ( 'NONE', #1222, #3272, #3009 ) ;
#642 = CARTESIAN_POINT ( 'NONE',  ( -66.99999999999997158, -5.000000000000000000, 44.49999999999999289 ) ) ;
#643 = VECTOR ( 'NONE', #2325, 1000.000000000000000 ) ;
#644 = TOROIDAL_SURFACE ( 'NONE', #1847, 3.299999999999999822, 0.2000000000000000111 ) ;
#645 = DIRECTION ( 'NONE',  ( -0.000000000000000000, 1.000000000000000000, -0.000000000000000000 ) ) ;
#646 = EDGE_CURVE ( 'NONE', #2761, #113, #2061, .T. ) ;
#647 = DIRECTION ( 'NONE',  ( -0.000000000000000000, -1.000000000000000000, -0.000000000000000000 ) ) ;
#648 = AXIS2_PLACEMENT_3D ( 'NONE', #1364, #592, #1637 ) ;
#649 = VECTOR ( 'NONE', #3280, 1000.000000000000000 ) ;
#650 = CARTESIAN_POINT ( 'NONE',  ( -66.99999999999997158, 0.000000000000000000, 41.99999999999999289 ) ) ;
#651 = EDGE_LOOP ( 'NONE', ( #1357, #2209 ) ) ;
#652 = LINE ( 'NONE', #1697, #534 ) ;
#653 = COLOUR_RGB ( '',0.8941176470588234615, 0.8941176470588234615, 0.8941176470588234615 ) ;
#654 = CARTESIAN_POINT ( 'NONE',  ( 44.99999999999999289, 56.00000000000000711, -10.00000000000000533 ) ) ;
#655 = ORIENTED_EDGE ( 'NONE', *, *, #3079, .T. ) ;
#656 = CARTESIAN_POINT ( 'NONE',  ( 44.99999999999999289, 45.00000000000000711, -12.00000000000000711 ) ) ;
#657 = DIRECTION ( 'NONE',  ( 0.000000000000000000, 0.000000000000000000, 1.000000000000000000 ) ) ;
#658 = EDGE_CURVE ( 'NONE', #223, #872, #1457, .T. ) ;
#659 = PRODUCT_CONTEXT ( 'NONE', #3321, 'mechanical' ) ;
#660 = DIRECTION ( 'NONE',  ( 1.000000000000000000, 0.000000000000000000, 0.000000000000000000 ) ) ;
#661 = CYLINDRICAL_SURFACE ( 'NONE', #314, 2.499999999999995115 ) ;
#662 = CYLINDRICAL_SURFACE ( 'NONE', #1528, 6.000000000000005329 ) ;
#663 = DIRECTION ( 'NONE',  ( 0.000000000000000000, 0.000000000000000000, 1.000000000000000000 ) ) ;
#664 = CARTESIAN_POINT ( 'NONE',  ( -49.99999999999999289, 136.9705627484771355, -4.999999999999995559 ) ) ;
#665 = DIRECTION ( 'NONE',  ( 0.000000000000000000, -0.000000000000000000, -1.000000000000000000 ) ) ;
#666 = EDGE_CURVE ( 'NONE', #617, #22, #2260, .T. ) ;
#667 = ORIENTED_EDGE ( 'NONE', *, *, #2408, .F. ) ;
#668 = DIRECTION ( 'NONE',  ( 0.000000000000000000, -0.5000000000000011102, -0.8660254037844379305 ) ) ;
#669 = PRODUCT_CONTEXT ( 'NONE', #112, 'mechanical' ) ;
#670 = EDGE_LOOP ( 'NONE', ( #138, #56, #2676, #1810 ) ) ;
#671 = DIRECTION ( 'NONE',  ( 0.000000000000000000, -0.000000000000000000, -1.000000000000000000 ) ) ;
#672 = CARTESIAN_POINT ( 'NONE',  ( 66.99999999999997158, -5.000000000000000000, -41.99999999999999289 ) ) ;
#673 = FACE_OUTER_BOUND ( 'NONE', #3258, .T. ) ;
#674 = EDGE_CURVE ( 'NONE', #2405, #2855, #370, .T. ) ;
#675 = CARTESIAN_POINT ( 'NONE',  ( -6.812556682370379590, 25.00000000000000000, 52.00000000000000000 ) ) ;
#676 = CARTESIAN_POINT ( 'NONE',  ( -40.00000000000000000, 117.0000000000000000, 5.000000000000004441 ) ) ;
#677 = PLANE ( 'NONE',  #2180 ) ;
#678 =( NAMED_UNIT ( * ) PLANE_ANGLE_UNIT ( ) SI_UNIT ( $, .RADIAN. ) );
#679 = ORIENTED_EDGE ( 'NONE', *, *, #3237, .T. ) ;
#680 = DIRECTION ( 'NONE',  ( -1.000000000000000000, -0.000000000000000000, 2.365532012695647326E-17 ) ) ;
#681 = SHAPE_DEFINITION_REPRESENTATION ( #1034, #1050 ) ;
#682 = ORIENTED_EDGE ( 'NONE', *, *, #392, .F. ) ;
#683 = CARTESIAN_POINT ( 'NONE',  ( 2.000000000000000000, -1.502314598737159426E-15, -1.535500000000000087 ) ) ;
#684 = VERTEX_POINT ( 'NONE', #490 ) ;
#685 = SHAPE_REPRESENTATION ( 'Base Enclosure^MAS-192', ( #3111 ), #1204 ) ;
#686 = CIRCLE ( 'NONE', #858, 2.500000000000009326 ) ;
#687 = FILL_AREA_STYLE_COLOUR ( '', #530 ) ;
#688 = DIRECTION ( 'NONE',  ( -0.000000000000000000, 1.000000000000000000, -0.000000000000000000 ) ) ;
#689 = VECTOR ( 'NONE', #1588, 1000.000000000000000 ) ;
#690 = CARTESIAN_POINT ( 'NONE',  ( -7.500000000000000000, 25.00000000000000000, 47.00000000000000000 ) ) ;
#691 = EDGE_CURVE ( 'NONE', #902, #38, #3333, .T. ) ;
#692 = ORIENTED_EDGE ( 'NONE', *, *, #3311, .F. ) ;
#693 = AXIS2_PLACEMENT_3D ( 'NONE', #3363, #1018, #2650 ) ;
#694 = LINE ( 'NONE', #1446, #867 ) ;
#695 = AXIS2_PLACEMENT_3D ( 'NONE', #1058, #2991, #2351 ) ;
#696 = DIRECTION ( 'NONE',  ( 0.000000000000000000, 0.000000000000000000, 1.000000000000000000 ) ) ;
#697 = TOROIDAL_SURFACE ( 'NONE', #1628, 2.200000000000001066, 0.2000000000000000111 ) ;
#698 = EDGE_CURVE ( 'NONE', #2833, #625, #1646, .T. ) ;
#699 = VERTEX_POINT ( 'NONE', #2973 ) ;
#700 = DIRECTION ( 'NONE',  ( -0.000000000000000000, 1.000000000000000000, 0.000000000000000000 ) ) ;
#701 = AXIS2_PLACEMENT_3D ( 'NONE', #1590, #222, #1270 ) ;
#702 = CIRCLE ( 'NONE', #1036, 2.499999999999995115 ) ;
#703 = CONTEXT_DEPENDENT_SHAPE_REPRESENTATION ( #2746, #2909 ) ;
#704 = PRESENTATION_LAYER_ASSIGNMENT (  '', '', ( #1905 ) ) ;
#705 = ORIENTED_EDGE ( 'NONE', *, *, #2348, .T. ) ;
#706 = CARTESIAN_POINT ( 'NONE',  ( -49.99999999999998579, 52.00000000000000711, 15.00000000000000888 ) ) ;
#707 = SURFACE_SIDE_STYLE ('',( #2258 ) ) ;
#708 = EDGE_CURVE ( 'NONE', #3353, #2365, #1789, .T. ) ;
#709 = ORIENTED_EDGE ( 'NONE', *, *, #2219, .T. ) ;
#710 = AXIS2_PLACEMENT_3D ( 'NONE', #312, #1354, #2397 ) ;
#711 = CARTESIAN_POINT ( 'NONE',  ( -66.99999999999997158, -6.000000000000000000, 41.99999999999999289 ) ) ;
#712 = CARTESIAN_POINT ( 'NONE',  ( 0.000000000000000000, 0.000000000000000000, 0.000000000000000000 ) ) ;
#713 = CARTESIAN_POINT ( 'NONE',  ( -50.00000000000000000, 117.0000000000000000, 5.000000000000004441 ) ) ;
#714 = SHAPE_REPRESENTATION ( 'vertical bar^MAS-192', ( #3111 ), #7 ) ;
#715 = DIRECTION ( 'NONE',  ( -1.000000000000000000, -0.000000000000000000, -0.000000000000000000 ) ) ;
#716 = DIRECTION ( 'NONE',  ( -0.000000000000000000, -1.000000000000000000, -0.000000000000000000 ) ) ;
#717 = PRESENTATION_STYLE_ASSIGNMENT (( #2810 ) ) ;
#718 = ORIENTED_EDGE ( 'NONE', *, *, #60, .T. ) ;
#719 = VERTEX_POINT ( 'NONE', #2682 ) ;
#720 = CARTESIAN_POINT ( 'NONE',  ( 55.00000000000004974, 120.0000000000000142, 5.000000000000004441 ) ) ;
#721 = EDGE_CURVE ( 'NONE', #468, #3203, #2942, .T. ) ;
#722 = CONTEXT_DEPENDENT_SHAPE_REPRESENTATION ( #851, #1332 ) ;
#723 = ORIENTED_EDGE ( 'NONE', *, *, #2943, .F. ) ;
#724 = CARTESIAN_POINT ( 'NONE',  ( -45.00000000000000000, 52.00000000000000711, -12.14999999999999503 ) ) ;
#725 = UNCERTAINTY_MEASURE_WITH_UNIT (LENGTH_MEASURE( 1.000000000000000082E-05 ), #364, 'distance_accuracy_value', 'NONE');
#726 = EDGE_LOOP ( 'NONE', ( #2242, #1959, #3250, #1072 ) ) ;
#727 = PRESENTATION_STYLE_ASSIGNMENT (( #469 ) ) ;
#728 = LINE ( 'NONE', #1509, #1455 ) ;
#729 = DIRECTION ( 'NONE',  ( -1.000000000000000000, 0.000000000000000000, 0.000000000000000000 ) ) ;
#730 = DIRECTION ( 'NONE',  ( 0.000000000000000000, 0.000000000000000000, 1.000000000000000000 ) ) ;
#731 = CARTESIAN_POINT ( 'NONE',  ( -66.99999999999997158, 0.000000000000000000, 41.99999999999999289 ) ) ;
#732 = EDGE_LOOP ( 'NONE', ( #224, #1699, #2690, #1975 ) ) ;
#733 = ORIENTED_EDGE ( 'NONE', *, *, #3213, .T. ) ;
#734 = FACE_OUTER_BOUND ( 'NONE', #1714, .T. ) ;
#735 = ORIENTED_EDGE ( 'NONE', *, *, #2411, .F. ) ;
#736 = EDGE_CURVE ( 'NONE', #1395, #436, #629, .T. ) ;
#737 = DIRECTION ( 'NONE',  ( 0.000000000000000000, -1.000000000000000000, 0.000000000000000000 ) ) ;
#738 = APPLICATION_CONTEXT ( 'automotive_design' ) ;
#739 = SHAPE_DEFINITION_REPRESENTATION ( #266, #3165 ) ;
#740 = VERTEX_POINT ( 'NONE', #1944 ) ;
#741 = EDGE_CURVE ( 'NONE', #2732, #2342, #2193, .T. ) ;
#742 = LINE ( 'NONE', #3123, #3097 ) ;
#743 = FILL_AREA_STYLE_COLOUR ( '', #3317 ) ;
#744 = DIRECTION ( 'NONE',  ( 0.000000000000000000, -0.000000000000000000, -1.000000000000000000 ) ) ;
#745 = DIRECTION ( 'NONE',  ( -1.000000000000000000, -0.000000000000000000, -0.000000000000000000 ) ) ;
#746 = CARTESIAN_POINT ( 'NONE',  ( -39.00000000000000000, 136.9705627484771355, 5.000000000000004441 ) ) ;
#747 =( LENGTH_UNIT ( ) NAMED_UNIT ( * ) SI_UNIT ( .MILLI., .METRE. ) );
#748 = ORIENTED_EDGE ( 'NONE', *, *, #283, .T. ) ;
#749 = VECTOR ( 'NONE', #1269, 1000.000000000000000 ) ;
#750 = EDGE_CURVE ( 'NONE', #624, #1751, #318, .T. ) ;
#751 = CONICAL_SURFACE ( 'NONE', #2655, 1.610000000000000098, 0.7853981633974652654 ) ;
#752 = EDGE_LOOP ( 'NONE', ( #2089, #1877, #2801, #609 ) ) ;
#753 = FACE_OUTER_BOUND ( 'NONE', #969, .T. ) ;
#754 = VECTOR ( 'NONE', #1951, 1000.000000000000000 ) ;
#755 = CONICAL_SURFACE ( 'NONE', #2177, 1.535500000000000087, 1.047197551196590748 ) ;
#756 = VERTEX_POINT ( 'NONE', #1175 ) ;
#757 = AXIS2_PLACEMENT_3D ( 'NONE', #1609, #2090, #2144 ) ;
#758 = CIRCLE ( 'NONE', #2664, 2.499999999999995115 ) ;
#759 = CARTESIAN_POINT ( 'NONE',  ( -39.99999999999999289, 52.00000000000000711, 15.00000000000000178 ) ) ;
#760 = UNCERTAINTY_MEASURE_WITH_UNIT (LENGTH_MEASURE( 1.000000000000000082E-05 ), #1279, 'distance_accuracy_value', 'NONE');
#761 = VECTOR ( 'NONE', #1874, 1000.000000000000000 ) ;
#762 = SURFACE_STYLE_USAGE ( .BOTH. , #1583 ) ;
#763 = ORIENTED_EDGE ( 'NONE', *, *, #1960, .F. ) ;
#764 = LINE ( 'NONE', #2586, #2546 ) ;
#765 = CIRCLE ( 'NONE', #2232, 2.149999999999999023 ) ;
#766 = LINE ( 'NONE', #1547, #529 ) ;
#767 = EDGE_CURVE ( 'NONE', #3340, #1840, #1842, .T. ) ;
#768 = CARTESIAN_POINT ( 'NONE',  ( -45.00000000000000000, 45.00000000000000711, -9.999999999999994671 ) ) ;
#769 = COLOUR_RGB ( '',0.8941176470588234615, 0.8941176470588234615, 0.8941176470588234615 ) ;
#770 = LINE ( 'NONE', #1806, #2815 ) ;
#771 = PLANE ( 'NONE',  #2227 ) ;
#772 = AXIS2_PLACEMENT_3D ( 'NONE', #3152, #1882, #2178 ) ;
#773 = CARTESIAN_POINT ( 'NONE',  ( 0.1999999999999987899, 0.000000000000000000, 0.000000000000000000 ) ) ;
#774 = VERTEX_POINT ( 'NONE', #2712 ) ;
#775 = ORIENTED_EDGE ( 'NONE', *, *, #886, .F. ) ;
#776 = DIRECTION ( 'NONE',  ( 1.000000000000000000, 0.000000000000000000, 0.000000000000000000 ) ) ;
#777 = EDGE_CURVE ( 'NONE', #3174, #895, #2769, .T. ) ;
#778 = ORIENTED_EDGE ( 'NONE', *, *, #535, .T. ) ;
#779 = PLANE ( 'NONE',  #1736 ) ;
#780 = ORIENTED_EDGE ( 'NONE', *, *, #1489, .F. ) ;
#781 = FACE_OUTER_BOUND ( 'NONE', #515, .T. ) ;
#782 = FACE_OUTER_BOUND ( 'NONE', #1028, .T. ) ;
#783 = EDGE_CURVE ( 'NONE', #3196, #489, #2960, .T. ) ;
#784 = DIRECTION ( 'NONE',  ( -0.000000000000000000, -0.000000000000000000, 1.000000000000000000 ) ) ;
#785 = PRODUCT_DEFINITION_SHAPE ( 'NONE', 'NONE',  #3375 ) ;
#786 = DIRECTION ( 'NONE',  ( -4.857225732735056709E-15, 0.000000000000000000, -1.000000000000000000 ) ) ;
#787 = VERTEX_POINT ( 'NONE', #580 ) ;
#788 = VERTEX_POINT ( 'NONE', #2445 ) ;
#789 = EDGE_CURVE ( 'NONE', #2683, #2543, #652, .T. ) ;
#790 = CARTESIAN_POINT ( 'NONE',  ( -50.00000000000000000, 136.9705627484771355, 5.000000000000004441 ) ) ;
#791 = EDGE_LOOP ( 'NONE', ( #1449, #2166, #1868, #3198 ) ) ;
#792 = LINE ( 'NONE', #1337, #2392 ) ;
#793 = EDGE_LOOP ( 'NONE', ( #299, #2023, #2312, #285 ) ) ;
#794 = EDGE_CURVE ( 'NONE', #1979, #575, #89, .T. ) ;
#795 =( LENGTH_UNIT ( ) NAMED_UNIT ( * ) SI_UNIT ( .MILLI., .METRE. ) );
#796 = FACE_BOUND ( 'NONE', #1865, .T. ) ;
#797 = LINE ( 'NONE', #543, #3212 ) ;
#798 = CARTESIAN_POINT ( 'NONE',  ( 0.000000000000000000, 25.00000000000000000, 47.00000000000000000 ) ) ;
#799 = CARTESIAN_POINT ( 'NONE',  ( -66.99999999999997158, -6.000000000000000000, 48.00000000000000000 ) ) ;
#800 = ORIENTED_EDGE ( 'NONE', *, *, #1328, .T. ) ;
#801 = VERTEX_POINT ( 'NONE', #857 ) ;
#802 = LINE ( 'NONE', #2887, #863 ) ;
#803 = AXIS2_PLACEMENT_3D ( 'NONE', #508, #1247, #1756 ) ;
#804 = ADVANCED_FACE ( 'NONE', ( #14 ), #755, .F. ) ;
#805 = AXIS2_PLACEMENT_3D ( 'NONE', #2415, #865, #2687 ) ;
#806 = ORIENTED_EDGE ( 'NONE', *, *, #2411, .T. ) ;
#807 = VECTOR ( 'NONE', #3083, 1000.000000000000000 ) ;
#808 = DIRECTION ( 'NONE',  ( 0.000000000000000000, 1.000000000000000000, -9.783878858594328898E-16 ) ) ;
#809 = CIRCLE ( 'NONE', #2548, 2.000000000000001776 ) ;
#810 = VECTOR ( 'NONE', #1384, 1000.000000000000000 ) ;
#811 = AXIS2_PLACEMENT_3D ( 'NONE', #2678, #2903, #1154 ) ;
#812 = ORIENTED_EDGE ( 'NONE', *, *, #2257, .F. ) ;
#813 = FACE_OUTER_BOUND ( 'NONE', #173, .T. ) ;
#814 = VECTOR ( 'NONE', #1147, 1000.000000000000000 ) ;
#815 = EDGE_CURVE ( 'NONE', #561, #719, #125, .T. ) ;
#816 = VECTOR ( 'NONE', #3084, 1000.000000000000000 ) ;
#817 = CARTESIAN_POINT ( 'NONE',  ( 75.00000000000000000, 50.00000000000000000, 50.00000000000000000 ) ) ;
#818 = DIRECTION ( 'NONE',  ( 0.000000000000000000, 0.000000000000000000, 1.000000000000000000 ) ) ;
#819 = LINE ( 'NONE', #3143, #488 ) ;
#820 = VERTEX_POINT ( 'NONE', #3202 ) ;
#821 = EDGE_LOOP ( 'NONE', ( #1255, #1521, #1611, #3308 ) ) ;
#822 = AXIS2_PLACEMENT_3D ( 'NONE', #1437, #385, #2221 ) ;
#823 = CARTESIAN_POINT ( 'NONE',  ( -40.00000000000000000, 120.0000000000000142, 5.000000000000004441 ) ) ;
#824 = VERTEX_POINT ( 'NONE', #1932 ) ;
#825 = EDGE_CURVE ( 'NONE', #3196, #2959, #3040, .T. ) ;
#826 = CYLINDRICAL_SURFACE ( 'NONE', #3105, 2.499999999999995115 ) ;
#827 = DIRECTION ( 'NONE',  ( 1.000000000000000000, 0.000000000000000000, 0.000000000000000000 ) ) ;
#828 = ORIENTED_EDGE ( 'NONE', *, *, #1481, .T. ) ;
#829 = CARTESIAN_POINT ( 'NONE',  ( 2.000000000000000000, 1.773042676681340524, -2.059984127722458425E-15 ) ) ;
#830 = FACE_OUTER_BOUND ( 'NONE', #2341, .T. ) ;
#831 =( REPRESENTATION_RELATIONSHIP ('NONE','NONE', #3165, #1286 ) REPRESENTATION_RELATIONSHIP_WITH_TRANSFORMATION ( #1033 )SHAPE_REPRESENTATION_RELATIONSHIP( ) );
#832 = DIRECTION ( 'NONE',  ( -0.000000000000000000, 1.000000000000000000, -0.000000000000000000 ) ) ;
#833 = CARTESIAN_POINT ( 'NONE',  ( -39.00000000000000000, 136.9705627484771355, -5.999999999999995559 ) ) ;
#834 = EDGE_LOOP ( 'NONE', ( #1103, #3022, #2540, #2748 ) ) ;
#835 = ORIENTED_EDGE ( 'NONE', *, *, #511, .F. ) ;
#836 = CARTESIAN_POINT ( 'NONE',  ( -39.99999999999999289, 52.00000000000000711, 15.00000000000000178 ) ) ;
#837 = FACE_OUTER_BOUND ( 'NONE', #1826, .T. ) ;
#838 = PRODUCT_DEFINITION_SHAPE ( 'NONE', 'NONE',  #3384 ) ;
#839 = ORIENTED_EDGE ( 'NONE', *, *, #241, .T. ) ;
#840 = DIRECTION ( 'NONE',  ( 0.000000000000000000, 0.000000000000000000, 1.000000000000000000 ) ) ;
#841 = LINE ( 'NONE', #533, #1409 ) ;
#842 = EDGE_CURVE ( 'NONE', #1605, #1570, #332, .T. ) ;
#843 = CARTESIAN_POINT ( 'NONE',  ( 0.000000000000000000, 0.000000000000000000, -83.99999999999998579 ) ) ;
#844 = ORIENTED_EDGE ( 'NONE', *, *, #736, .F. ) ;
#845 = PLANE ( 'NONE',  #2875 ) ;
#846 = ADVANCED_FACE ( 'NONE', ( #75 ), #1125, .T. ) ;
#847 = CYLINDRICAL_SURFACE ( 'NONE', #805, 2.499999999999995115 ) ;
#848 = CARTESIAN_POINT ( 'NONE',  ( -45.00000000000000000, 50.00000000000000000, -9.999999999999994671 ) ) ;
#849 = AXIS2_PLACEMENT_3D ( 'NONE', #134, #663, #1707 ) ;
#850 = ORIENTED_EDGE ( 'NONE', *, *, #794, .T. ) ;
#851 =( REPRESENTATION_RELATIONSHIP ('NONE','NONE', #3165, #107 ) REPRESENTATION_RELATIONSHIP_WITH_TRANSFORMATION ( #2022 )SHAPE_REPRESENTATION_RELATIONSHIP( ) );
#852 = ORIENTED_EDGE ( 'NONE', *, *, #503, .F. ) ;
#853 = CARTESIAN_POINT ( 'NONE',  ( -66.99999999999997158, -6.000000000000000000, 41.99999999999999289 ) ) ;
#854 = FACE_OUTER_BOUND ( 'NONE', #1573, .T. ) ;
#855 = ADVANCED_FACE ( 'NONE', ( #1918 ), #614, .F. ) ;
#856 = ORIENTED_EDGE ( 'NONE', *, *, #1712, .T. ) ;
#857 = CARTESIAN_POINT ( 'NONE',  ( -44.99999999999999289, 50.00000000000000000, 8.000000000000003553 ) ) ;
#858 = AXIS2_PLACEMENT_3D ( 'NONE', #3313, #2011, #3055 ) ;
#859 = VERTEX_POINT ( 'NONE', #2036 ) ;
#860 = CONICAL_SURFACE ( 'NONE', #693, 7.250000000000000000, 0.08726646259971666819 ) ;
#861 = AXIS2_PLACEMENT_3D ( 'NONE', #1652, #290, #1635 ) ;
#862 = DIRECTION ( 'NONE',  ( 0.000000000000000000, -1.000000000000000000, 0.000000000000000000 ) ) ;
#863 = VECTOR ( 'NONE', #1523, 1000.000000000000114 ) ;
#864 = SURFACE_STYLE_FILL_AREA ( #3179 ) ;
#865 = DIRECTION ( 'NONE',  ( -0.000000000000000000, 1.000000000000000000, -0.000000000000000000 ) ) ;
#866 = CARTESIAN_POINT ( 'NONE',  ( -49.99999999999999289, 120.0000000000000142, -4.999999999999995559 ) ) ;
#867 = VECTOR ( 'NONE', #1248, 1000.000000000000000 ) ;
#868 = EDGE_CURVE ( 'NONE', #2623, #2345, #2510, .T. ) ;
#869 = CARTESIAN_POINT ( 'NONE',  ( -40.00000000000000000, 120.0000000000000142, -4.999999999999995559 ) ) ;
#870 = AXIS2_PLACEMENT_3D ( 'NONE', #3071, #2860, #2062 ) ;
#871 = VERTEX_POINT ( 'NONE', #929 ) ;
#872 = VERTEX_POINT ( 'NONE', #1235 ) ;
#873 = DIRECTION ( 'NONE',  ( 0.000000000000000000, -1.224646799147353207E-16, 1.000000000000000000 ) ) ;
#874 = COLOUR_RGB ( '',0.8941176470588234615, 0.8941176470588234615, 0.8941176470588234615 ) ;
#875 = DIRECTION ( 'NONE',  ( 0.000000000000000000, 0.000000000000000000, 1.000000000000000000 ) ) ;
#876 = DIRECTION ( 'NONE',  ( 0.000000000000000000, 0.5150380749100514910, 0.8571673007021138879 ) ) ;
#877 = EDGE_LOOP ( 'NONE', ( #13, #2657 ) ) ;
#878 = DIRECTION ( 'NONE',  ( 0.000000000000000000, 0.000000000000000000, 1.000000000000000000 ) ) ;
#879 = ADVANCED_FACE ( 'NONE', ( #3023 ), #2238, .T. ) ;
#880 = VERTEX_POINT ( 'NONE', #2292 ) ;
#881 = LINE ( 'NONE', #3259, #1625 ) ;
#882 = PRESENTATION_STYLE_ASSIGNMENT (( #80 ) ) ;
#883 = DIRECTION ( 'NONE',  ( -0.000000000000000000, -0.000000000000000000, 1.000000000000000000 ) ) ;
#884 = DIRECTION ( 'NONE',  ( -0.000000000000000000, 1.000000000000000000, -0.000000000000000000 ) ) ;
#885 = DIRECTION ( 'NONE',  ( 0.000000000000000000, 0.000000000000000000, 1.000000000000000000 ) ) ;
#886 = EDGE_CURVE ( 'NONE', #2365, #2834, #2218, .T. ) ;
#887 = VERTEX_POINT ( 'NONE', #1746 ) ;
#888 = ORIENTED_EDGE ( 'NONE', *, *, #2262, .T. ) ;
#889 = CARTESIAN_POINT ( 'NONE',  ( 0.1999999999999987899, 4.041334437186265510E-16, -3.299999999999999822 ) ) ;
#890 = CARTESIAN_POINT ( 'NONE',  ( 2.000000000000000000, -0.8865213383406694847, 1.535500000000001419 ) ) ;
#891 = EDGE_CURVE ( 'NONE', #1277, #3215, #1450, .T. ) ;
#892 = EDGE_LOOP ( 'NONE', ( #1598, #2085, #61, #1335, #2189 ) ) ;
#893 = DIRECTION ( 'NONE',  ( -0.000000000000000000, 1.000000000000000000, -0.000000000000000000 ) ) ;
#894 = APPLICATION_PROTOCOL_DEFINITION ( 'draft international standard', 'automotive_design', 1998, #1678 ) ;
#895 = VERTEX_POINT ( 'NONE', #463 ) ;
#896 = DIRECTION ( 'NONE',  ( 0.000000000000000000, 0.000000000000000000, -1.000000000000000000 ) ) ;
#897 =( LENGTH_UNIT ( ) NAMED_UNIT ( * ) SI_UNIT ( .MILLI., .METRE. ) );
#898 = EDGE_CURVE ( 'NONE', #872, #1926, #2783, .T. ) ;
#899 = CARTESIAN_POINT ( 'NONE',  ( 0.000000000000000000, -1.773042676681341856, 2.276824562219559311E-15 ) ) ;
#900 = DIRECTION ( 'NONE',  ( 0.000000000000000000, 0.000000000000000000, -1.000000000000000000 ) ) ;
#901 = CARTESIAN_POINT ( 'NONE',  ( -49.99999999999999289, 117.0000000000000000, -4.999999999999995559 ) ) ;
#902 = VERTEX_POINT ( 'NONE', #720 ) ;
#903 = DIRECTION ( 'NONE',  ( 0.000000000000000000, -0.4999999999999989453, 0.8660254037844391517 ) ) ;
#904 = FACE_OUTER_BOUND ( 'NONE', #85, .T. ) ;
#905 = EDGE_LOOP ( 'NONE', ( #1623, #1912, #1670 ) ) ;
#906 = DIRECTION ( 'NONE',  ( 0.000000000000000000, -1.000000000000000000, 0.000000000000000000 ) ) ;
#907 = EDGE_CURVE ( 'NONE', #38, #2342, #2800, .T. ) ;
#908 = ORIENTED_EDGE ( 'NONE', *, *, #2303, .F. ) ;
#909 = CARTESIAN_POINT ( 'NONE',  ( -66.99999999999997158, 0.000000000000000000, 41.99999999999999289 ) ) ;
#910 = VECTOR ( 'NONE', #1496, 1000.000000000000000 ) ;
#911 =( LENGTH_UNIT ( ) NAMED_UNIT ( * ) SI_UNIT ( .MILLI., .METRE. ) );
#912 = VECTOR ( 'NONE', #2702, 1000.000000000000000 ) ;
#913 = AXIS2_PLACEMENT_3D ( 'NONE', #3141, #2879, #1165 ) ;
#914 = FACE_OUTER_BOUND ( 'NONE', #200, .T. ) ;
#915 = CARTESIAN_POINT ( 'NONE',  ( -66.99999999999997158, -6.000000000000000000, 41.99999999999999289 ) ) ;
#916 = APPLICATION_CONTEXT ( 'automotive_design' ) ;
#917 = CIRCLE ( 'NONE', #1141, 7.500000000000000000 ) ;
#918 = ADVANCED_FACE ( 'NONE', ( #2479 ), #1899, .T. ) ;
#919 = VECTOR ( 'NONE', #2073, 1000.000000000000000 ) ;
#920 = DIRECTION ( 'NONE',  ( 0.000000000000000000, 0.000000000000000000, -1.000000000000000000 ) ) ;
#921 = VECTOR ( 'NONE', #3175, 1000.000000000000000 ) ;
#922 = AXIS2_PLACEMENT_3D ( 'NONE', #1606, #2937, #610 ) ;
#923 = CARTESIAN_POINT ( 'NONE',  ( 0.000000000000000000, 0.000000000000000000, 0.000000000000000000 ) ) ;
#924 = CARTESIAN_POINT ( 'NONE',  ( -50.00000000000000000, 136.9705627484771355, 6.000000000000004441 ) ) ;
#925 = VECTOR ( 'NONE', #3, 1000.000000000000000 ) ;
#926 = FILL_AREA_STYLE ('',( #2289 ) ) ;
#927 = ORIENTED_EDGE ( 'NONE', *, *, #2482, .T. ) ;
#928 = AXIS2_PLACEMENT_3D ( 'NONE', #2519, #1495, #920 ) ;
#929 = CARTESIAN_POINT ( 'NONE',  ( -66.99999999999997158, -6.000000000000000000, 39.49999999999998579 ) ) ;
#930 = ADVANCED_BREP_SHAPE_REPRESENTATION ( '', ( #2021, #3111 ), #2 ) ;
#931 = PRESENTATION_LAYER_ASSIGNMENT (  '', '', ( #985 ) ) ;
#932 = SHAPE_DEFINITION_REPRESENTATION ( #2611, #1286 ) ;
#933 = ORIENTED_EDGE ( 'NONE', *, *, #283, .F. ) ;
#934 = EDGE_CURVE ( 'NONE', #1751, #1843, #449, .T. ) ;
#935 = PLANE ( 'NONE',  #2763 ) ;
#936 = SHAPE_REPRESENTATION ( 'switch^MAS-192', ( #3111 ), #2779 ) ;
#937 = CARTESIAN_POINT ( 'NONE',  ( 0.000000000000000000, 25.00000000000000000, 47.00000000000000000 ) ) ;
#938 = CARTESIAN_POINT ( 'NONE',  ( -66.99999999999997158, -8.000000000000000000, 44.50000000000000711 ) ) ;
#939 = DIRECTION ( 'NONE',  ( -0.000000000000000000, 1.000000000000000000, -0.000000000000000000 ) ) ;
#940 = VERTEX_POINT ( 'NONE', #1436 ) ;
#941 = CARTESIAN_POINT ( 'NONE',  ( -40.00000000000000000, 52.00000000000000711, -4.999999999999996447 ) ) ;
#942 = DIRECTION ( 'NONE',  ( -0.000000000000000000, -0.000000000000000000, 1.000000000000000000 ) ) ;
#943 = ORIENTED_EDGE ( 'NONE', *, *, #459, .F. ) ;
#944 = CARTESIAN_POINT ( 'NONE',  ( 66.99999999999997158, -5.000000000000000000, 41.99999999999999289 ) ) ;
#945 = PRODUCT_CONTEXT ( 'NONE', #1857, 'mechanical' ) ;
#946 = PRODUCT_DEFINITION_SHAPE ( 'NONE', 'NONE',  #3378 ) ;
#947 = ORIENTED_EDGE ( 'NONE', *, *, #1080, .T. ) ;
#948 = CARTESIAN_POINT ( 'NONE',  ( -50.00000000000000000, 136.9705627484771355, 5.000000000000004441 ) ) ;
#949 = EDGE_CURVE ( 'NONE', #1041, #608, #430, .T. ) ;
#950 = ORIENTED_EDGE ( 'NONE', *, *, #1226, .F. ) ;
#951 = DIRECTION ( 'NONE',  ( 0.000000000000000000, -1.000000000000000000, 0.000000000000000000 ) ) ;
#952 = CARTESIAN_POINT ( 'NONE',  ( 66.99999999999997158, 0.000000000000000000, 41.99999999999999289 ) ) ;
#953 = ADVANCED_FACE ( 'NONE', ( #2745 ), #2269, .T. ) ;
#954 = LINE ( 'NONE', #1988, #1308 ) ;
#955 = DIRECTION ( 'NONE',  ( 1.000000000000000000, 0.000000000000000000, 0.000000000000000000 ) ) ;
#956 = CARTESIAN_POINT ( 'NONE',  ( 45.00000000000000000, 45.00000000000000711, 7.999999999999992895 ) ) ;
#957 = DIRECTION ( 'NONE',  ( 0.000000000000000000, 0.000000000000000000, 1.000000000000000000 ) ) ;
#958 = ORIENTED_EDGE ( 'NONE', *, *, #1431, .F. ) ;
#959 = CARTESIAN_POINT ( 'NONE',  ( -44.99999999999999289, 52.00000000000000711, 12.15000000000000391 ) ) ;
#960 = ADVANCED_FACE ( 'NONE', ( #734 ), #412, .T. ) ;
#961 = APPLICATION_PROTOCOL_DEFINITION ( 'draft international standard', 'automotive_design', 1998, #2725 ) ;
#962 = ORIENTED_EDGE ( 'NONE', *, *, #1226, .T. ) ;
#963 = PLANE ( 'NONE',  #1092 ) ;
#964 = EDGE_LOOP ( 'NONE', ( #1584, #2798, #775, #3184, #2217 ) ) ;
#965 = AXIS2_PLACEMENT_3D ( 'NONE', #3127, #3072, #1786 ) ;
#966 = DIRECTION ( 'NONE',  ( 0.000000000000000000, 0.000000000000000000, -1.000000000000000000 ) ) ;
#967 = LINE ( 'NONE', #419, #649 ) ;
#968 = LINE ( 'NONE', #2315, #981 ) ;
#969 = EDGE_LOOP ( 'NONE', ( #2568, #3228 ) ) ;
#970 = EDGE_CURVE ( 'NONE', #2106, #1968, #809, .T. ) ;
#971 = AXIS2_PLACEMENT_3D ( 'NONE', #585, #862, #1870 ) ;
#972 = LINE ( 'NONE', #1433, #1410 ) ;
#973 = AXIS2_PLACEMENT_3D ( 'NONE', #1897, #840, #2668 ) ;
#974 = CARTESIAN_POINT ( 'NONE',  ( -66.99999999999997158, -6.000000000000000000, 48.00000000000000000 ) ) ;
#975 = AXIS2_PLACEMENT_3D ( 'NONE', #261, #211, #2079 ) ;
#976 = AXIS2_PLACEMENT_3D ( 'NONE', #2536, #446, #903 ) ;
#977 = ORIENTED_EDGE ( 'NONE', *, *, #416, .F. ) ;
#978 = DIRECTION ( 'NONE',  ( 0.000000000000000000, 0.000000000000000000, 1.000000000000000000 ) ) ;
#979 = CIRCLE ( 'NONE', #2716, 0.2000000000000000944 ) ;
#980 = CIRCLE ( 'NONE', #2557, 2.499999999999995115 ) ;
#981 = VECTOR ( 'NONE', #1533, 1000.000000000000000 ) ;
#982 = EDGE_LOOP ( 'NONE', ( #2278, #548, #2419 ) ) ;
#983 = ADVANCED_FACE ( 'NONE', ( #2525 ), #1725, .F. ) ;
#984 = FACE_BOUND ( 'NONE', #1823, .T. ) ;
#985 = STYLED_ITEM ( 'NONE', ( #3121 ), #1506 ) ;
#986 = APPLICATION_CONTEXT ( 'automotive_design' ) ;
#987 = EDGE_LOOP ( 'NONE', ( #2562, #705, #1656, #127 ) ) ;
#988 = PRODUCT_DEFINITION_FORMATION_WITH_SPECIFIED_SOURCE ( 'ANY', '', #1577, .NOT_KNOWN. ) ;
#989 = DIRECTION ( 'NONE',  ( 0.000000000000000000, 0.000000000000000000, 1.000000000000000000 ) ) ;
#990 = CARTESIAN_POINT ( 'NONE',  ( -45.00000000000000000, 52.00000000000000711, -9.999999999999994671 ) ) ;
#991 = FACE_OUTER_BOUND ( 'NONE', #1558, .T. ) ;
#992 = ADVANCED_FACE ( 'NONE', ( #1471 ), #3303, .F. ) ;
#993 = ORIENTED_EDGE ( 'NONE', *, *, #16, .F. ) ;
#994 = ORIENTED_EDGE ( 'NONE', *, *, #2107, .T. ) ;
#995 = DIRECTION ( 'NONE',  ( 0.000000000000000000, -0.000000000000000000, 1.000000000000000000 ) ) ;
#996 = PRODUCT_DEFINITION_CONTEXT ( 'detailed design', #2030, 'design' ) ;
#997 = EDGE_CURVE ( 'NONE', #2026, #1965, #204, .T. ) ;
#998 = CONTEXT_DEPENDENT_SHAPE_REPRESENTATION ( #2420, #2765 ) ;
#999 = ORIENTED_EDGE ( 'NONE', *, *, #24, .F. ) ;
#1000 = DIRECTION ( 'NONE',  ( 0.000000000000000000, -1.000000000000000000, 0.000000000000000000 ) ) ;
#1001 = ORIENTED_EDGE ( 'NONE', *, *, #2906, .T. ) ;
#1002 = CARTESIAN_POINT ( 'NONE',  ( -66.99999999999997158, -6.000000000000000000, 35.99999999999999289 ) ) ;
#1003 = CARTESIAN_POINT ( 'NONE',  ( 0.000000000000000000, -1.773042676681341856, 2.276824562219559311E-15 ) ) ;
#1004 = ADVANCED_FACE ( 'NONE', ( #3132 ), #294, .F. ) ;
#1005 = FACE_BOUND ( 'NONE', #506, .T. ) ;
#1006 = DIRECTION ( 'NONE',  ( -0.000000000000000000, -1.000000000000000000, -0.000000000000000000 ) ) ;
#1007 = DIRECTION ( 'NONE',  ( 0.000000000000000000, 0.000000000000000000, 1.000000000000000000 ) ) ;
#1008 = SURFACE_SIDE_STYLE ('',( #2114 ) ) ;
#1009 = ORIENTED_EDGE ( 'NONE', *, *, #767, .T. ) ;
#1010 = ORIENTED_EDGE ( 'NONE', *, *, #2997, .F. ) ;
#1011 = FACE_OUTER_BOUND ( 'NONE', #1227, .T. ) ;
#1012 = ITEM_DEFINED_TRANSFORMATION ( 'NONE', 'NONE', #2726,  #3111 ) ;
#1013 = ORIENTED_EDGE ( 'NONE', *, *, #1945, .F. ) ;
#1014 = ADVANCED_FACE ( 'NONE', ( #753 ), #1776, .F. ) ;
#1015 = DIRECTION ( 'NONE',  ( 1.000000000000000000, 0.000000000000000000, -0.000000000000000000 ) ) ;
#1016 = EDGE_LOOP ( 'NONE', ( #943, #568, #1889, #718 ) ) ;
#1017 = DIRECTION ( 'NONE',  ( -6.938893903907228378E-16, -0.000000000000000000, 1.000000000000000000 ) ) ;
#1018 = DIRECTION ( 'NONE',  ( -0.000000000000000000, -0.000000000000000000, -1.000000000000000000 ) ) ;
#1019 = DIRECTION ( 'NONE',  ( 0.000000000000000000, 0.000000000000000000, 1.000000000000000000 ) ) ;
#1020 = DIRECTION ( 'NONE',  ( 0.000000000000000000, 0.000000000000000000, 1.000000000000000000 ) ) ;
#1021 = EDGE_CURVE ( 'NONE', #84, #309, #1844, .T. ) ;
#1022 = LINE ( 'NONE', #2356, #1097 ) ;
#1023 = AXIS2_PLACEMENT_3D ( 'NONE', #2606, #272, #1316 ) ;
#1024 = LINE ( 'NONE', #1569, #2229 ) ;
#1025 = ORIENTED_EDGE ( 'NONE', *, *, #2262, .F. ) ;
#1026 = VECTOR ( 'NONE', #1683, 1000.000000000000000 ) ;
#1027 = VECTOR ( 'NONE', #876, 999.9999999999998863 ) ;
#1028 = EDGE_LOOP ( 'NONE', ( #1469, #2196, #1120, #2571 ) ) ;
#1029 = DIRECTION ( 'NONE',  ( 1.000000000000000000, 0.000000000000000000, 0.000000000000000000 ) ) ;
#1030 = PRODUCT_DEFINITION_CONTEXT ( 'detailed design', #2377, 'design' ) ;
#1031 = AXIS2_PLACEMENT_3D ( 'NONE', #650, #1156, #1434 ) ;
#1032 = AXIS2_PLACEMENT_3D ( 'NONE', #1228, #2298, #1782 ) ;
#1033 = ITEM_DEFINED_TRANSFORMATION ( 'NONE', 'NONE', #3057,  #3111 ) ;
#1034 = PRODUCT_DEFINITION_SHAPE ( 'NONE', 'NONE',  #2584 ) ;
#1035 = ORIENTED_EDGE ( 'NONE', *, *, #1068, .T. ) ;
#1036 = AXIS2_PLACEMENT_3D ( 'NONE', #186, #423, #3006 ) ;
#1037 = LINE ( 'NONE', #724, #1684 ) ;
#1038 = UNCERTAINTY_MEASURE_WITH_UNIT (LENGTH_MEASURE( 1.000000000000000082E-05 ), #333, 'distance_accuracy_value', 'NONE');
#1039 = VECTOR ( 'NONE', #942, 1000.000000000000000 ) ;
#1040 = ADVANCED_FACE ( 'NONE', ( #1011 ), #1517, .T. ) ;
#1041 = VERTEX_POINT ( 'NONE', #2814 ) ;
#1042 = DIRECTION ( 'NONE',  ( 0.000000000000000000, 0.000000000000000000, -1.000000000000000000 ) ) ;
#1043 = ADVANCED_FACE ( 'NONE', ( #2321 ), #2375, .T. ) ;
#1044 = DIRECTION ( 'NONE',  ( -1.000000000000000000, 0.000000000000000000, -0.000000000000000000 ) ) ;
#1045 = CARTESIAN_POINT ( 'NONE',  ( -45.00000000000000000, 50.00000000000000000, -12.14999999999999503 ) ) ;
#1046 = DIRECTION ( 'NONE',  ( -0.000000000000000000, 1.000000000000000000, -0.000000000000000000 ) ) ;
#1047 = DIRECTION ( 'NONE',  ( 0.000000000000000000, -1.000000000000000000, 0.000000000000000000 ) ) ;
#1048 = ORIENTED_EDGE ( 'NONE', *, *, #3063, .F. ) ;
#1049 = EDGE_LOOP ( 'NONE', ( #2630, #1234 ) ) ;
#1050 = SHAPE_REPRESENTATION ( 'Support Feet^MAS-192', ( #3111 ), #2 ) ;
#1051 = LINE ( 'NONE', #2087, #2501 ) ;
#1052 = ADVANCED_FACE ( 'NONE', ( #1083 ), #37, .T. ) ;
#1053 = ITEM_DEFINED_TRANSFORMATION ( 'NONE', 'NONE', #2949,  #3111 ) ;
#1054 = VERTEX_POINT ( 'NONE', #1322 ) ;
#1055 = CARTESIAN_POINT ( 'NONE',  ( 75.00000000000000000, 50.00000000000000000, 50.00000000000000000 ) ) ;
#1056 =( LENGTH_UNIT ( ) NAMED_UNIT ( * ) SI_UNIT ( .MILLI., .METRE. ) );
#1057 = ORIENTED_EDGE ( 'NONE', *, *, #2408, .T. ) ;
#1058 = CARTESIAN_POINT ( 'NONE',  ( -66.99999999999997158, -5.000000000000000000, 41.99999999999999289 ) ) ;
#1059 = LINE ( 'NONE', #231, #2064 ) ;
#1060 = DIRECTION ( 'NONE',  ( 0.000000000000000000, -1.000000000000000000, 0.000000000000000000 ) ) ;
#1061 = DIRECTION ( 'NONE',  ( 1.000000000000000000, 0.000000000000000000, 0.000000000000000000 ) ) ;
#1062 = CARTESIAN_POINT ( 'NONE',  ( -50.00000000000000000, 120.0000000000000142, 5.000000000000004441 ) ) ;
#1063 = ADVANCED_FACE ( 'NONE', ( #2051, #2102, #3091 ), #256, .T. ) ;
#1064 = ORIENTED_EDGE ( 'NONE', *, *, #137, .T. ) ;
#1065 = ORIENTED_EDGE ( 'NONE', *, *, #3024, .T. ) ;
#1066 = CARTESIAN_POINT ( 'NONE',  ( 0.000000000000000000, 50.00000000000000000, 0.000000000000000000 ) ) ;
#1067 = ORIENTED_EDGE ( 'NONE', *, *, #2876, .F. ) ;
#1068 = EDGE_CURVE ( 'NONE', #3353, #2100, #802, .T. ) ;
#1069 = DIRECTION ( 'NONE',  ( 0.000000000000000000, 0.000000000000000000, -1.000000000000000000 ) ) ;
#1070 = UNCERTAINTY_MEASURE_WITH_UNIT (LENGTH_MEASURE( 1.000000000000000082E-05 ), #2231, 'distance_accuracy_value', 'NONE');
#1071 = SURFACE_STYLE_FILL_AREA ( #2669 ) ;
#1072 = ORIENTED_EDGE ( 'NONE', *, *, #1390, .F. ) ;
#1073 =( REPRESENTATION_RELATIONSHIP ('NONE','NONE', #3165, #1050 ) REPRESENTATION_RELATIONSHIP_WITH_TRANSFORMATION ( #2272 )SHAPE_REPRESENTATION_RELATIONSHIP( ) );
#1074 = CARTESIAN_POINT ( 'NONE',  ( -40.00000000000000000, 52.00000000000000711, -5.999999999999995559 ) ) ;
#1075 = DIRECTION ( 'NONE',  ( -1.000000000000000000, -0.000000000000000000, -0.000000000000000000 ) ) ;
#1076 = VECTOR ( 'NONE', #955, 1000.000000000000000 ) ;
#1077 = CARTESIAN_POINT ( 'NONE',  ( 4.200000000000001954, 0.000000000000000000, -2.200000000000001066 ) ) ;
#1078 = LINE ( 'NONE', #2111, #2438 ) ;
#1079 = FILL_AREA_STYLE ('',( #2372 ) ) ;
#1080 = EDGE_CURVE ( 'NONE', #2072, #1203, #1299, .T. ) ;
#1081 = ORIENTED_EDGE ( 'NONE', *, *, #2552, .T. ) ;
#1082 = ORIENTED_EDGE ( 'NONE', *, *, #2552, .F. ) ;
#1083 = FACE_OUTER_BOUND ( 'NONE', #237, .T. ) ;
#1084 = AXIS2_PLACEMENT_3D ( 'NONE', #251, #2301, #2316 ) ;
#1085 = AXIS2_PLACEMENT_3D ( 'NONE', #1615, #3162, #1636 ) ;
#1086 = VECTOR ( 'NONE', #1803, 1000.000000000000000 ) ;
#1087 = ORIENTED_EDGE ( 'NONE', *, *, #304, .F. ) ;
#1088 = PRESENTATION_LAYER_ASSIGNMENT (  '', '', ( #3211 ) ) ;
#1089 = CARTESIAN_POINT ( 'NONE',  ( -45.00000000000000000, 52.00000000000000711, -12.14999999999999503 ) ) ;
#1090 = AXIS2_PLACEMENT_3D ( 'NONE', #2616, #2119, #3356 ) ;
#1091 =( NAMED_UNIT ( * ) SI_UNIT ( $, .STERADIAN. ) SOLID_ANGLE_UNIT ( ) );
#1092 = AXIS2_PLACEMENT_3D ( 'NONE', #1999, #3328, #808 ) ;
#1093 = CIRCLE ( 'NONE', #2992, 2.499999999999995115 ) ;
#1094 = ORIENTED_EDGE ( 'NONE', *, *, #1564, .T. ) ;
#1095 = CARTESIAN_POINT ( 'NONE',  ( -66.99999999999997158, 0.000000000000000000, 41.99999999999999289 ) ) ;
#1096 = COLOUR_RGB ( '',0.8941176470588234615, 0.8941176470588234615, 0.8941176470588234615 ) ;
#1097 = VECTOR ( 'NONE', #1788, 1000.000000000000000 ) ;
#1098 = VECTOR ( 'NONE', #471, 1000.000000000000000 ) ;
#1099 = CARTESIAN_POINT ( 'NONE',  ( 10.00000000000000178, 0.000000000000000000, 0.000000000000000000 ) ) ;
#1100 = DIRECTION ( 'NONE',  ( -0.000000000000000000, 1.000000000000000000, -0.000000000000000000 ) ) ;
#1101 =( GEOMETRIC_REPRESENTATION_CONTEXT ( 3 ) GLOBAL_UNCERTAINTY_ASSIGNED_CONTEXT ( ( #2836 ) ) GLOBAL_UNIT_ASSIGNED_CONTEXT ( ( #1780, #1627, #284 ) ) REPRESENTATION_CONTEXT ( 'NONE', 'WORKASPACE' ) );
#1102 = LINE ( 'NONE', #3195, #761 ) ;
#1103 = ORIENTED_EDGE ( 'NONE', *, *, #1913, .F. ) ;
#1104 = ORIENTED_EDGE ( 'NONE', *, *, #2997, .T. ) ;
#1105 = AXIS2_PLACEMENT_3D ( 'NONE', #616, #1919, #827 ) ;
#1106 = DIRECTION ( 'NONE',  ( 0.000000000000000000, 0.000000000000000000, 1.000000000000000000 ) ) ;
#1107 = ADVANCED_FACE ( 'NONE', ( #225 ), #3217, .F. ) ;
#1108 = DIRECTION ( 'NONE',  ( -0.000000000000000000, 1.000000000000000000, -0.000000000000000000 ) ) ;
#1109 = ORIENTED_EDGE ( 'NONE', *, *, #2475, .F. ) ;
#1110 = CARTESIAN_POINT ( 'NONE',  ( 66.99999999999997158, -5.000000000000000000, 41.99999999999999289 ) ) ;
#1111 = EDGE_CURVE ( 'NONE', #1240, #1126, #500, .T. ) ;
#1112 =( NAMED_UNIT ( * ) SI_UNIT ( $, .STERADIAN. ) SOLID_ANGLE_UNIT ( ) );
#1113 = ORIENTED_EDGE ( 'NONE', *, *, #2350, .F. ) ;
#1114 = CARTESIAN_POINT ( 'NONE',  ( -44.99999999999999289, 50.00000000000000000, 10.00000000000000533 ) ) ;
#1115 = DIRECTION ( 'NONE',  ( 0.000000000000000000, 0.000000000000000000, 1.000000000000000000 ) ) ;
#1116 = DIRECTION ( 'NONE',  ( -1.000000000000000000, -0.000000000000000000, -0.000000000000000000 ) ) ;
#1117 = FACE_OUTER_BOUND ( 'NONE', #791, .T. ) ;
#1118 = EDGE_CURVE ( 'NONE', #2239, #78, #1287, .T. ) ;
#1119 = LINE ( 'NONE', #1150, #2339 ) ;
#1120 = ORIENTED_EDGE ( 'NONE', *, *, #1987, .F. ) ;
#1121 = ORIENTED_EDGE ( 'NONE', *, *, #1492, .T. ) ;
#1122 = FACE_OUTER_BOUND ( 'NONE', #1948, .T. ) ;
#1123 = CARTESIAN_POINT ( 'NONE',  ( -39.99999999999999289, 52.00000000000000711, 15.00000000000000178 ) ) ;
#1124 = ORIENTED_EDGE ( 'NONE', *, *, #1387, .T. ) ;
#1125 = CYLINDRICAL_SURFACE ( 'NONE', #1572, 3.500000000000000000 ) ;
#1126 = VERTEX_POINT ( 'NONE', #1812 ) ;
#1127 = ADVANCED_FACE ( 'NONE', ( #2854 ), #514, .F. ) ;
#1128 = DIRECTION ( 'NONE',  ( 0.000000000000000000, -0.4999999999999991118, 0.8660254037844391517 ) ) ;
#1129 = SHAPE_REPRESENTATION_RELATIONSHIP ( 'NONE' , 'NONE' ,  #685, #479 ) ;
#1130 = CARTESIAN_POINT ( 'NONE',  ( 45.00000000000000000, 45.00000000000000711, 11.99999999999999645 ) ) ;
#1131 = FACE_OUTER_BOUND ( 'NONE', #2670, .T. ) ;
#1132 = DIRECTION ( 'NONE',  ( -0.000000000000000000, -1.000000000000000000, -0.000000000000000000 ) ) ;
#1133 = ORIENTED_EDGE ( 'NONE', *, *, #777, .T. ) ;
#1134 = EDGE_CURVE ( 'NONE', #2834, #940, #1051, .T. ) ;
#1135 = ORIENTED_EDGE ( 'NONE', *, *, #611, .T. ) ;
#1136 = DIRECTION ( 'NONE',  ( -1.000000000000000000, -0.000000000000000000, -0.000000000000000000 ) ) ;
#1137 = DIRECTION ( 'NONE',  ( -0.000000000000000000, 1.000000000000000000, -0.000000000000000000 ) ) ;
#1138 = ORIENTED_EDGE ( 'NONE', *, *, #1885, .T. ) ;
#1139 = DIRECTION ( 'NONE',  ( -0.000000000000000000, 1.000000000000000000, -0.000000000000000000 ) ) ;
#1140 = ORIENTED_EDGE ( 'NONE', *, *, #443, .T. ) ;
#1141 = AXIS2_PLACEMENT_3D ( 'NONE', #1375, #92, #1884 ) ;
#1142 = VECTOR ( 'NONE', #1386, 1000.000000000000000 ) ;
#1143 = CARTESIAN_POINT ( 'NONE',  ( 2.000000000000000000, 0.000000000000000000, 0.000000000000000000 ) ) ;
#1144 = ADVANCED_FACE ( 'NONE', ( #1657 ), #2918, .F. ) ;
#1145 = AXIS2_PLACEMENT_3D ( 'NONE', #853, #2462, #1878 ) ;
#1146 = CARTESIAN_POINT ( 'NONE',  ( 4.200000000000001954, 0.000000000000000000, 0.000000000000000000 ) ) ;
#1147 = DIRECTION ( 'NONE',  ( -1.000000000000000000, -0.000000000000000000, -0.000000000000000000 ) ) ;
#1148 = AXIS2_PLACEMENT_3D ( 'NONE', #836, #1891, #2662 ) ;
#1149 = EDGE_CURVE ( 'NONE', #1763, #1570, #375, .T. ) ;
#1150 = CARTESIAN_POINT ( 'NONE',  ( -75.00000000000000000, 50.00000000000000000, 50.00000000000000000 ) ) ;
#1151 = CIRCLE ( 'NONE', #2617, 2.499999999999995115 ) ;
#1152 = EDGE_LOOP ( 'NONE', ( #2290, #341, #2481, #2578 ) ) ;
#1153 = ORIENTED_EDGE ( 'NONE', *, *, #2802, .T. ) ;
#1154 = DIRECTION ( 'NONE',  ( 0.000000000000000000, -0.000000000000000000, -1.000000000000000000 ) ) ;
#1155 = MECHANICAL_DESIGN_GEOMETRIC_PRESENTATION_REPRESENTATION (  '', ( #384 ), #2399 ) ;
#1156 = DIRECTION ( 'NONE',  ( 0.000000000000000000, -1.000000000000000000, 0.000000000000000000 ) ) ;
#1157 = AXIS2_PLACEMENT_3D ( 'NONE', #111, #160, #413 ) ;
#1158 = ORIENTED_EDGE ( 'NONE', *, *, #374, .F. ) ;
#1159 = CARTESIAN_POINT ( 'NONE',  ( 2.000000000000000000, 1.773042676681340524, -2.059984127722458425E-15 ) ) ;
#1160 = EDGE_CURVE ( 'NONE', #2976, #1539, #72, .T. ) ;
#1161 = APPLICATION_PROTOCOL_DEFINITION ( 'draft international standard', 'automotive_design', 1998, #986 ) ;
#1162 = ORIENTED_EDGE ( 'NONE', *, *, #1845, .F. ) ;
#1163 = CARTESIAN_POINT ( 'NONE',  ( -45.00000000000000000, 50.00000000000000000, -9.999999999999994671 ) ) ;
#1164 =( LENGTH_UNIT ( ) NAMED_UNIT ( * ) SI_UNIT ( .MILLI., .METRE. ) );
#1165 = DIRECTION ( 'NONE',  ( 0.000000000000000000, 0.000000000000000000, 1.000000000000000000 ) ) ;
#1166 = CARTESIAN_POINT ( 'NONE',  ( -45.00000000000000000, 45.00000000000000711, -7.999999999999992895 ) ) ;
#1167 = APPLICATION_CONTEXT ( 'automotive_design' ) ;
#1168 = DIRECTION ( 'NONE',  ( 1.049727191138620668E-16, 0.5150380749100514910, -0.8571673007021138879 ) ) ;
#1169 = ORIENTED_EDGE ( 'NONE', *, *, #1118, .F. ) ;
#1170 = ORIENTED_EDGE ( 'NONE', *, *, #2436, .T. ) ;
#1171 = ADVANCED_FACE ( 'NONE', ( #2692, #2203 ), #3199, .F. ) ;
#1172 = DIRECTION ( 'NONE',  ( 0.000000000000000000, 0.000000000000000000, -1.000000000000000000 ) ) ;
#1173 = DIRECTION ( 'NONE',  ( 0.000000000000000000, 0.000000000000000000, 1.000000000000000000 ) ) ;
#1174 = ORIENTED_EDGE ( 'NONE', *, *, #1747, .T. ) ;
#1175 = CARTESIAN_POINT ( 'NONE',  ( -39.00000000000000000, 117.0000000000000000, 6.000000000000004441 ) ) ;
#1176 = ORIENTED_EDGE ( 'NONE', *, *, #2378, .F. ) ;
#1177 = CYLINDRICAL_SURFACE ( 'NONE', #2116, 2.499999999999995115 ) ;
#1178 = CARTESIAN_POINT ( 'NONE',  ( 45.00000000000000000, 45.00000000000000711, 11.99999999999999645 ) ) ;
#1179 = CARTESIAN_POINT ( 'NONE',  ( 66.99999999999997158, 0.000000000000000000, 41.99999999999999289 ) ) ;
#1180 = FACE_OUTER_BOUND ( 'NONE', #3074, .T. ) ;
#1181 = CARTESIAN_POINT ( 'NONE',  ( -40.00000000000000000, 50.00000000000000000, 5.000000000000004441 ) ) ;
#1182 = EDGE_CURVE ( 'NONE', #1041, #2643, #356, .T. ) ;
#1183 = CARTESIAN_POINT ( 'NONE',  ( 44.99999999999999289, 45.00000000000000711, -12.00000000000000711 ) ) ;
#1184 = ORIENTED_EDGE ( 'NONE', *, *, #2784, .T. ) ;
#1185 = DIRECTION ( 'NONE',  ( -1.000000000000000000, 0.000000000000000000, 0.000000000000000000 ) ) ;
#1186 = DIRECTION ( 'NONE',  ( 0.000000000000000000, 0.000000000000000000, 1.000000000000000000 ) ) ;
#1187 = EDGE_LOOP ( 'NONE', ( #806, #2969 ) ) ;
#1188 = FACE_OUTER_BOUND ( 'NONE', #2799, .T. ) ;
#1189 =( NAMED_UNIT ( * ) PLANE_ANGLE_UNIT ( ) SI_UNIT ( $, .RADIAN. ) );
#1190 = AXIS2_PLACEMENT_3D ( 'NONE', #2752, #2724, #2230 ) ;
#1191 = AXIS2_PLACEMENT_3D ( 'NONE', #672, #951, #1412 ) ;
#1192 = FACE_OUTER_BOUND ( 'NONE', #1049, .T. ) ;
#1193 = CARTESIAN_POINT ( 'NONE',  ( -40.00000000000000000, 117.0000000000000000, -5.999999999999995559 ) ) ;
#1194 = AXIS2_PLACEMENT_3D ( 'NONE', #2910, #569, #1983 ) ;
#1195 = VECTOR ( 'NONE', #680, 1000.000000000000000 ) ;
#1196 = FACE_OUTER_BOUND ( 'NONE', #2237, .T. ) ;
#1197 = VECTOR ( 'NONE', #1069, 1000.000000000000000 ) ;
#1198 = CIRCLE ( 'NONE', #3106, 2.000000000000001776 ) ;
#1199 = DIRECTION ( 'NONE',  ( -0.000000000000000000, 1.000000000000000000, -0.000000000000000000 ) ) ;
#1200 = DIRECTION ( 'NONE',  ( -1.000000000000000000, 0.000000000000000000, -0.000000000000000000 ) ) ;
#1201 = CIRCLE ( 'NONE', #2613, 2.499999999999995115 ) ;
#1202 = CYLINDRICAL_SURFACE ( 'NONE', #373, 2.149999999999999023 ) ;
#1203 = VERTEX_POINT ( 'NONE', #2190 ) ;
#1204 =( GEOMETRIC_REPRESENTATION_CONTEXT ( 3 ) GLOBAL_UNCERTAINTY_ASSIGNED_CONTEXT ( ( #1038 ) ) GLOBAL_UNIT_ASSIGNED_CONTEXT ( ( #333, #1819, #2430 ) ) REPRESENTATION_CONTEXT ( 'NONE', 'WORKASPACE' ) );
#1205 = DIRECTION ( 'NONE',  ( 0.000000000000000000, 0.000000000000000000, 1.000000000000000000 ) ) ;
#1206 = EDGE_CURVE ( 'NONE', #436, #859, #210, .T. ) ;
#1207 = PRODUCT_DEFINITION_CONTEXT ( 'detailed design', #287, 'design' ) ;
#1208 = MECHANICAL_DESIGN_GEOMETRIC_PRESENTATION_REPRESENTATION (  '', ( #1468 ), #3054 ) ;
#1209 = ORIENTED_EDGE ( 'NONE', *, *, #666, .T. ) ;
#1210 =( REPRESENTATION_RELATIONSHIP ('NONE','NONE', #3165, #1050 ) REPRESENTATION_RELATIONSHIP_WITH_TRANSFORMATION ( #1053 )SHAPE_REPRESENTATION_RELATIONSHIP( ) );
#1211 = EDGE_CURVE ( 'NONE', #787, #190, #765, .T. ) ;
#1212 = CARTESIAN_POINT ( 'NONE',  ( 0.1999999999999987899, 0.000000000000000000, 3.500000000000000000 ) ) ;
#1213 =( NAMED_UNIT ( * ) PLANE_ANGLE_UNIT ( ) SI_UNIT ( $, .RADIAN. ) );
#1214 = CARTESIAN_POINT ( 'NONE',  ( 0.000000000000000000, 25.00000000000000000, 52.00000000000000000 ) ) ;
#1215 = DIRECTION ( 'NONE',  ( -0.000000000000000000, 1.000000000000000000, -0.000000000000000000 ) ) ;
#1216 = CARTESIAN_POINT ( 'NONE',  ( -66.99999999999997158, -5.000000000000000000, 39.50000000000000000 ) ) ;
#1217 = FACE_BOUND ( 'NONE', #2427, .T. ) ;
#1218 = ADVANCED_FACE ( 'NONE', ( #2439 ), #1576, .F. ) ;
#1219 = DIRECTION ( 'NONE',  ( -0.000000000000000000, 1.345283343056720273E-15, 1.000000000000000000 ) ) ;
#1220 = DIRECTION ( 'NONE',  ( 1.049727191138620668E-16, 0.5150380749100514910, -0.8571673007021138879 ) ) ;
#1221 = ORIENTED_EDGE ( 'NONE', *, *, #868, .T. ) ;
#1222 = CARTESIAN_POINT ( 'NONE',  ( -40.00000000000000000, 136.9705627484771355, 5.000000000000004441 ) ) ;
#1223 = DIRECTION ( 'NONE',  ( 0.000000000000000000, 0.000000000000000000, 1.000000000000000000 ) ) ;
#1224 = ORIENTED_EDGE ( 'NONE', *, *, #2353, .F. ) ;
#1225 = CARTESIAN_POINT ( 'NONE',  ( -54.99999999999995026, 130.0000000000000000, 5.000000000000004441 ) ) ;
#1226 = EDGE_CURVE ( 'NONE', #2291, #801, #51, .T. ) ;
#1227 = EDGE_LOOP ( 'NONE', ( #723, #1351, #1260, #502 ) ) ;
#1228 = CARTESIAN_POINT ( 'NONE',  ( 2.000000000000000000, 0.000000000000000000, 0.000000000000000000 ) ) ;
#1229 = CARTESIAN_POINT ( 'NONE',  ( -66.99999999999997158, 0.000000000000000000, 44.50000000000000711 ) ) ;
#1230 = CARTESIAN_POINT ( 'NONE',  ( 2.000000000000000000, -0.8865213383406694847, 1.535500000000001419 ) ) ;
#1231 = DIRECTION ( 'NONE',  ( 0.000000000000000000, 0.000000000000000000, 1.000000000000000000 ) ) ;
#1232 = DIRECTION ( 'NONE',  ( 0.000000000000000000, 0.000000000000000000, -1.000000000000000000 ) ) ;
#1233 = ADVANCED_FACE ( 'NONE', ( #122, #103, #377, #1642, #577 ), #1864, .T. ) ;
#1234 = ORIENTED_EDGE ( 'NONE', *, *, #3013, .F. ) ;
#1235 = CARTESIAN_POINT ( 'NONE',  ( 2.000000000000000000, -1.329782007511005837, 0.7677500000000023750 ) ) ;
#1236 = AXIS2_PLACEMENT_3D ( 'NONE', #2505, #3032, #1989 ) ;
#1237 = ORIENTED_EDGE ( 'NONE', *, *, #741, .T. ) ;
#1238 = DIRECTION ( 'NONE',  ( 0.000000000000000000, 0.5000000000000011102, 0.8660254037844379305 ) ) ;
#1239 = SURFACE_STYLE_FILL_AREA ( #3099 ) ;
#1240 = VERTEX_POINT ( 'NONE', #2645 ) ;
#1241 = CARTESIAN_POINT ( 'NONE',  ( -44.99999999999999289, 50.00000000000000000, 12.00000000000000711 ) ) ;
#1242 = FILL_AREA_STYLE ('',( #15 ) ) ;
#1243 = ADVANCED_FACE ( 'NONE', ( #2970 ), #101, .T. ) ;
#1244 = CIRCLE ( 'NONE', #379, 2.500000000000009326 ) ;
#1245 =( GEOMETRIC_REPRESENTATION_CONTEXT ( 3 ) GLOBAL_UNCERTAINTY_ASSIGNED_CONTEXT ( ( #2091 ) ) GLOBAL_UNIT_ASSIGNED_CONTEXT ( ( #3069, #2845, #230 ) ) REPRESENTATION_CONTEXT ( 'NONE', 'WORKASPACE' ) );
#1246 = CARTESIAN_POINT ( 'NONE',  ( -66.99999999999997158, -5.000000000000000000, -41.99999999999999289 ) ) ;
#1247 = DIRECTION ( 'NONE',  ( -0.000000000000000000, 1.000000000000000000, -0.000000000000000000 ) ) ;
#1248 = DIRECTION ( 'NONE',  ( -1.000000000000000000, -0.000000000000000000, -0.000000000000000000 ) ) ;
#1249 = AXIS2_PLACEMENT_3D ( 'NONE', #174, #2762, #189 ) ;
#1250 = EDGE_CURVE ( 'NONE', #2460, #1968, #308, .T. ) ;
#1251 = DIRECTION ( 'NONE',  ( 0.000000000000000000, -1.000000000000000000, 0.000000000000000000 ) ) ;
#1252 = CIRCLE ( 'NONE', #3161, 2.499999999999995115 ) ;
#1253 = VECTOR ( 'NONE', #2781, 1000.000000000000000 ) ;
#1254 = ORIENTED_EDGE ( 'NONE', *, *, #2848, .F. ) ;
#1255 = ORIENTED_EDGE ( 'NONE', *, *, #1304, .F. ) ;
#1256 = DIRECTION ( 'NONE',  ( -1.000000000000000000, -0.000000000000000000, -0.000000000000000000 ) ) ;
#1257 = AXIS2_PLACEMENT_3D ( 'NONE', #3233, #884, #818 ) ;
#1258 = CONTEXT_DEPENDENT_SHAPE_REPRESENTATION ( #1210, #3295 ) ;
#1259=STYLED_ITEM('',(#3415),#3171);
#1260 = ORIENTED_EDGE ( 'NONE', *, *, #1908, .F. ) ;
#1261 = ADVANCED_FACE ( 'NONE', ( #1122 ), #3186, .T. ) ;
#1262 = CARTESIAN_POINT ( 'NONE',  ( -66.99999999999997158, -6.000000000000000000, 37.49999999999998579 ) ) ;
#1263 =( GEOMETRIC_REPRESENTATION_CONTEXT ( 3 ) GLOBAL_UNCERTAINTY_ASSIGNED_CONTEXT ( ( #2493 ) ) GLOBAL_UNIT_ASSIGNED_CONTEXT ( ( #1560, #1854, #1112 ) ) REPRESENTATION_CONTEXT ( 'NONE', 'WORKASPACE' ) );
#1264 = SHAPE_REPRESENTATION_RELATIONSHIP ( 'NONE' , 'NONE' ,  #107, #1 ) ;
#1265 = EDGE_LOOP ( 'NONE', ( #1109, #1927 ) ) ;
#1266 = CARTESIAN_POINT ( 'NONE',  ( 44.99999999999999289, 45.00000000000000711, -10.00000000000000533 ) ) ;
#1267 = DIRECTION ( 'NONE',  ( -0.000000000000000000, -1.000000000000000000, -0.000000000000000000 ) ) ;
#1268 = LINE ( 'NONE', #817, #2058 ) ;
#1269 = DIRECTION ( 'NONE',  ( -1.000000000000000000, 0.000000000000000000, 0.000000000000000000 ) ) ;
#1270 = DIRECTION ( 'NONE',  ( 0.000000000000000000, 0.000000000000000000, 1.000000000000000000 ) ) ;
#1271 = ADVANCED_FACE ( 'NONE', ( #328 ), #1368, .T. ) ;
#1272 = ORIENTED_EDGE ( 'NONE', *, *, #1111, .F. ) ;
#1273 = ORIENTED_EDGE ( 'NONE', *, *, #1950, .F. ) ;
#1274 = VERTEX_POINT ( 'NONE', #2422 ) ;
#1275 = DIRECTION ( 'NONE',  ( 0.000000000000000000, 0.000000000000000000, 1.000000000000000000 ) ) ;
#1276 = EDGE_CURVE ( 'NONE', #21, #887, #2069, .T. ) ;
#1277 = VERTEX_POINT ( 'NONE', #3219 ) ;
#1278 = CARTESIAN_POINT ( 'NONE',  ( 2.000000000000000000, 1.329782007511006281, 0.7677499999999984892 ) ) ;
#1279 =( LENGTH_UNIT ( ) NAMED_UNIT ( * ) SI_UNIT ( .MILLI., .METRE. ) );
#1280 = DIRECTION ( 'NONE',  ( -0.000000000000000000, 1.000000000000000000, -0.000000000000000000 ) ) ;
#1281 = CARTESIAN_POINT ( 'NONE',  ( 2.000000000000000000, 1.773042676681340524, -2.059984127722458425E-15 ) ) ;
#1282 = CARTESIAN_POINT ( 'NONE',  ( 66.99999999999997158, 0.000000000000000000, -44.49999999999999289 ) ) ;
#1283 = LINE ( 'NONE', #276, #2395 ) ;
#1284 = ORIENTED_EDGE ( 'NONE', *, *, #1600, .F. ) ;
#1285 = ORIENTED_EDGE ( 'NONE', *, *, #1701, .F. ) ;
#1286 = SHAPE_REPRESENTATION ( 'socket head cap screw_iso_ISO 4762 M4 x 6 - 6N', ( #3111 ), #1101 ) ;
#1287 = LINE ( 'NONE', #3371, #485 ) ;
#1288 = EDGE_CURVE ( 'NONE', #801, #2291, #537, .T. ) ;
#1289 = CONTEXT_DEPENDENT_SHAPE_REPRESENTATION ( #2163, #3164 ) ;
#1290 = ORIENTED_EDGE ( 'NONE', *, *, #750, .F. ) ;
#1291 = DIRECTION ( 'NONE',  ( -0.000000000000000000, 1.000000000000000000, -0.000000000000000000 ) ) ;
#1292 = ORIENTED_EDGE ( 'NONE', *, *, #241, .F. ) ;
#1293 = CYLINDRICAL_SURFACE ( 'NONE', #637, 6.000000000000005329 ) ;
#1294 = AXIS2_PLACEMENT_3D ( 'NONE', #1281, #1061, #1770 ) ;
#1295 = DIRECTION ( 'NONE',  ( 2.365532012695647018E-17, -0.000000000000000000, 1.000000000000000000 ) ) ;
#1296 = CARTESIAN_POINT ( 'NONE',  ( 45.00000000000000000, 45.00000000000000711, 9.999999999999994671 ) ) ;
#1297 = VERTEX_POINT ( 'NONE', #1740 ) ;
#1298 = ORIENTED_EDGE ( 'NONE', *, *, #3357, .T. ) ;
#1299 = LINE ( 'NONE', #2564, #919 ) ;
#1300 = CIRCLE ( 'NONE', #2446, 2.499999999999995115 ) ;
#1301 = VECTOR ( 'NONE', #399, 1000.000000000000000 ) ;
#1302 = CONTEXT_DEPENDENT_SHAPE_REPRESENTATION ( #831, #52 ) ;
#1303 = ORIENTED_EDGE ( 'NONE', *, *, #2303, .T. ) ;
#1304 = EDGE_CURVE ( 'NONE', #448, #2972, #702, .T. ) ;
#1305 = CIRCLE ( 'NONE', #431, 3.500000000000000000 ) ;
#1306 = AXIS2_PLACEMENT_3D ( 'NONE', #1915, #2391, #1172 ) ;
#1307 = DIRECTION ( 'NONE',  ( 0.000000000000000000, 0.8660254037844380415, -0.5000000000000012212 ) ) ;
#1308 = VECTOR ( 'NONE', #444, 1000.000000000000000 ) ;
#1309 = FILL_AREA_STYLE_COLOUR ( '', #653 ) ;
#1310 = ORIENTED_EDGE ( 'NONE', *, *, #133, .T. ) ;
#1311 = EDGE_CURVE ( 'NONE', #625, #2623, #2265, .T. ) ;
#1312 = DIRECTION ( 'NONE',  ( -0.08715574274765836016, -1.067350013832299517E-17, -0.9961946980917455452 ) ) ;
#1313 = STYLED_ITEM ( 'NONE', ( #2530 ), #516 ) ;
#1314 = CARTESIAN_POINT ( 'NONE',  ( -66.99999999999997158, 0.000000000000000000, 37.49999999999998579 ) ) ;
#1315 = PLANE ( 'NONE',  #542 ) ;
#1316 = DIRECTION ( 'NONE',  ( 0.000000000000000000, 0.000000000000000000, -1.000000000000000000 ) ) ;
#1317 = CARTESIAN_POINT ( 'NONE',  ( -66.99999999999997158, -8.000000000000000000, 41.99999999999999289 ) ) ;
#1318 = DIRECTION ( 'NONE',  ( -0.000000000000000000, -1.000000000000000000, -0.000000000000000000 ) ) ;
#1319 = VERTEX_POINT ( 'NONE', #2476 ) ;
#1320 = EDGE_CURVE ( 'NONE', #2398, #2976, #1694, .T. ) ;
#1321 = ORIENTED_EDGE ( 'NONE', *, *, #1727, .T. ) ;
#1322 = CARTESIAN_POINT ( 'NONE',  ( 2.000000000000000000, -0.8865213383406694847, 1.535500000000001419 ) ) ;
#1323 = ORIENTED_EDGE ( 'NONE', *, *, #1607, .F. ) ;
#1324 = LINE ( 'NONE', #62, #1197 ) ;
#1325 = DIRECTION ( 'NONE',  ( 0.000000000000000000, 0.000000000000000000, 1.000000000000000000 ) ) ;
#1326 = ORIENTED_EDGE ( 'NONE', *, *, #970, .F. ) ;
#1327 = CYLINDRICAL_SURFACE ( 'NONE', #2001, 2.000000000000001776 ) ;
#1328 = EDGE_CURVE ( 'NONE', #2543, #1126, #2741, .T. ) ;
#1329 = FACE_OUTER_BOUND ( 'NONE', #1663, .T. ) ;
#1330 = CARTESIAN_POINT ( 'NONE',  ( -40.00000000000000000, 117.0000000000000000, 5.000000000000004441 ) ) ;
#1331 = CARTESIAN_POINT ( 'NONE',  ( 0.000000000000000000, 1.773042676681340524, -2.059984127722458425E-15 ) ) ;
#1332 = PRODUCT_DEFINITION_SHAPE ( 'NONE', 'NONE',  #3377 ) ;
#1333 = PLANE ( 'NONE',  #1901 ) ;
#1334 = ORIENTED_EDGE ( 'NONE', *, *, #3070, .T. ) ;
#1335 = ORIENTED_EDGE ( 'NONE', *, *, #898, .T. ) ;
#1336 = ORIENTED_EDGE ( 'NONE', *, *, #220, .T. ) ;
#1337 = CARTESIAN_POINT ( 'NONE',  ( -44.99999999999999289, 50.00000000000000000, 8.000000000000003553 ) ) ;
#1338 = ORIENTED_EDGE ( 'NONE', *, *, #2015, .F. ) ;
#1339 = DIRECTION ( 'NONE',  ( 0.000000000000000000, 0.000000000000000000, 1.000000000000000000 ) ) ;
#1340 = FACE_OUTER_BOUND ( 'NONE', #1529, .T. ) ;
#1341 = ADVANCED_FACE ( 'NONE', ( #3314 ), #2522, .F. ) ;
#1342 = DIRECTION ( 'NONE',  ( 0.000000000000000000, 0.000000000000000000, -1.000000000000000000 ) ) ;
#1343 = CARTESIAN_POINT ( 'NONE',  ( 66.99999999999997158, -5.000000000000000000, -41.99999999999999289 ) ) ;
#1344 = ORIENTED_EDGE ( 'NONE', *, *, #1991, .T. ) ;
#1345 = VERTEX_POINT ( 'NONE', #1961 ) ;
#1346 = ADVANCED_FACE ( 'NONE', ( #2985 ), #1990, .T. ) ;
#1347 = CARTESIAN_POINT ( 'NONE',  ( -45.00000000000000000, 45.00000000000000711, -7.999999999999992895 ) ) ;
#1348 = CIRCLE ( 'NONE', #1892, 2.149999999999999023 ) ;
#1349 = AXIS2_PLACEMENT_3D ( 'NONE', #1179, #3296, #1937 ) ;
#1350 = AXIS2_PLACEMENT_3D ( 'NONE', #1099, #3160, #587 ) ;
#1351 = ORIENTED_EDGE ( 'NONE', *, *, #1206, .T. ) ;
#1352 = DIRECTION ( 'NONE',  ( -0.000000000000000000, 1.000000000000000000, -0.000000000000000000 ) ) ;
#1353 = AXIS2_PLACEMENT_3D ( 'NONE', #3038, #700, #2019 ) ;
#1354 = DIRECTION ( 'NONE',  ( 0.000000000000000000, 0.000000000000000000, 1.000000000000000000 ) ) ;
#1355 = VECTOR ( 'NONE', #1530, 1000.000000000000000 ) ;
#1356 = CONICAL_SURFACE ( 'NONE', #3163, 2.000000000000001776, 1.029744258676657642 ) ;
#1357 = ORIENTED_EDGE ( 'NONE', *, *, #32, .F. ) ;
#1358 = ADVANCED_FACE ( 'NONE', ( #135 ), #171, .F. ) ;
#1359 = CARTESIAN_POINT ( 'NONE',  ( -44.99999999999999289, 45.00000000000000711, 8.000000000000003553 ) ) ;
#1360 = PRESENTATION_LAYER_ASSIGNMENT (  '', '', ( #2503 ) ) ;
#1361 =( NAMED_UNIT ( * ) SI_UNIT ( $, .STERADIAN. ) SOLID_ANGLE_UNIT ( ) );
#1362 = DIRECTION ( 'NONE',  ( 0.000000000000000000, 0.000000000000000000, 1.000000000000000000 ) ) ;
#1363 = CARTESIAN_POINT ( 'NONE',  ( -31.74999999999995737, 0.000000000000000000, 3.500000000000000000 ) ) ;
#1364 = CARTESIAN_POINT ( 'NONE',  ( 9.610000000000013642, 0.000000000000000000, 0.000000000000000000 ) ) ;
#1365 = ORIENTED_EDGE ( 'NONE', *, *, #1211, .F. ) ;
#1366 = ORIENTED_EDGE ( 'NONE', *, *, #3013, .T. ) ;
#1367 = PRODUCT_DEFINITION_FORMATION_WITH_SPECIFIED_SOURCE ( 'ANY', '', #510, .NOT_KNOWN. ) ;
#1368 = PLANE ( 'NONE',  #2826 ) ;
#1369 = EDGE_CURVE ( 'NONE', #1054, #2078, #694, .T. ) ;
#1370 = DIRECTION ( 'NONE',  ( 0.000000000000000000, 1.000000000000000000, -0.000000000000000000 ) ) ;
#1371 = ORIENTED_EDGE ( 'NONE', *, *, #1970, .T. ) ;
#1372 = CARTESIAN_POINT ( 'NONE',  ( -54.99999999999995026, 130.0000000000000000, -4.999999999999997335 ) ) ;
#1373 = DIRECTION ( 'NONE',  ( 1.000000000000000000, 0.000000000000000000, 0.000000000000000000 ) ) ;
#1374 = ORIENTED_EDGE ( 'NONE', *, *, #1970, .F. ) ;
#1375 = CARTESIAN_POINT ( 'NONE',  ( 0.000000000000000000, 25.00000000000000000, 47.00000000000000000 ) ) ;
#1376 = PRODUCT_RELATED_PRODUCT_CATEGORY ( 'part', '', ( #2551 ) ) ;
#1377 = SURFACE_SIDE_STYLE ('',( #864 ) ) ;
#1378 = CARTESIAN_POINT ( 'NONE',  ( -51.00000000000000000, 117.0000000000000000, -5.999999999999995559 ) ) ;
#1379 = DIRECTION ( 'NONE',  ( -0.000000000000000000, -1.000000000000000000, -0.000000000000000000 ) ) ;
#1380 = PLANE ( 'NONE',  #1687 ) ;
#1381 = ORIENTED_EDGE ( 'NONE', *, *, #1551, .T. ) ;
#1382 = ORIENTED_EDGE ( 'NONE', *, *, #1311, .F. ) ;
#1383 = DIRECTION ( 'NONE',  ( 0.000000000000000000, 0.000000000000000000, -1.000000000000000000 ) ) ;
#1384 = DIRECTION ( 'NONE',  ( 1.000000000000000000, 0.000000000000000000, 0.000000000000000000 ) ) ;
#1385 = ORIENTED_EDGE ( 'NONE', *, *, #545, .T. ) ;
#1386 = DIRECTION ( 'NONE',  ( -0.000000000000000000, -1.000000000000000000, -0.000000000000000000 ) ) ;
#1387 = EDGE_CURVE ( 'NONE', #2306, #2732, #972, .T. ) ;
#1388 =( NAMED_UNIT ( * ) PLANE_ANGLE_UNIT ( ) SI_UNIT ( $, .RADIAN. ) );
#1389 = EDGE_LOOP ( 'NONE', ( #1221, #2124, #120, #3042 ) ) ;
#1390 = EDGE_CURVE ( 'NONE', #108, #2833, #3056, .T. ) ;
#1391 = DIRECTION ( 'NONE',  ( -0.000000000000000000, 1.000000000000000000, -0.000000000000000000 ) ) ;
#1392 = DIRECTION ( 'NONE',  ( 0.000000000000000000, 0.000000000000000000, 1.000000000000000000 ) ) ;
#1393 = CARTESIAN_POINT ( 'NONE',  ( 66.99999999999997158, 0.000000000000000000, -39.50000000000000000 ) ) ;
#1394 = CYLINDRICAL_SURFACE ( 'NONE', #3329, 4.500000000000010658 ) ;
#1395 = VERTEX_POINT ( 'NONE', #1757 ) ;
#1396 = EDGE_LOOP ( 'NONE', ( #1863, #2412, #1553, #462, #3275 ) ) ;
#1397 = EDGE_CURVE ( 'NONE', #3137, #2623, #1940, .T. ) ;
#1398 = DIRECTION ( 'NONE',  ( -0.000000000000000000, 1.000000000000000000, -0.000000000000000000 ) ) ;
#1399 = CARTESIAN_POINT ( 'NONE',  ( -31.74999999999995737, 0.000000000000000000, 0.000000000000000000 ) ) ;
#1400 = CIRCLE ( 'NONE', #3092, 2.149999999999999023 ) ;
#1401 = EDGE_LOOP ( 'NONE', ( #1831, #519, #3370 ) ) ;
#1402 = DIRECTION ( 'NONE',  ( 0.000000000000000000, 0.000000000000000000, -1.000000000000000000 ) ) ;
#1403 = VECTOR ( 'NONE', #470, 999.9999999999998863 ) ;
#1404 = AXIS2_PLACEMENT_3D ( 'NONE', #638, #1429, #1972 ) ;
#1405 = PRODUCT_CONTEXT ( 'NONE', #986, 'mechanical' ) ;
#1406 = VERTEX_POINT ( 'NONE', #2234 ) ;
#1407 = AXIS2_PLACEMENT_3D ( 'NONE', #3287, #995, #156 ) ;
#1408 = CARTESIAN_POINT ( 'NONE',  ( -75.00000000000000000, 50.00000000000000000, 50.00000000000000000 ) ) ;
#1409 = VECTOR ( 'NONE', #1582, 1000.000000000000000 ) ;
#1410 = VECTOR ( 'NONE', #410, 1000.000000000000000 ) ;
#1411 = EDGE_CURVE ( 'NONE', #480, #774, #460, .T. ) ;
#1412 = DIRECTION ( 'NONE',  ( 0.000000000000000000, 0.000000000000000000, -1.000000000000000000 ) ) ;
#1413 = DIRECTION ( 'NONE',  ( -1.000000000000000000, -0.000000000000000000, -0.000000000000000000 ) ) ;
#1414 = AXIS2_PLACEMENT_3D ( 'NONE', #559, #2370, #351 ) ;
#1415 = CARTESIAN_POINT ( 'NONE',  ( -31.74999999999995737, 2.449293598294707893E-16, -2.000000000000000888 ) ) ;
#1416 = MECHANICAL_DESIGN_GEOMETRIC_PRESENTATION_REPRESENTATION (  '', ( #1905 ), #2128 ) ;
#1417 = ORIENTED_EDGE ( 'NONE', *, *, #2205, .F. ) ;
#1418 = CARTESIAN_POINT ( 'NONE',  ( -66.99999999999997158, -8.000000000000000000, 35.99999999999999289 ) ) ;
#1419 = DIRECTION ( 'NONE',  ( -0.000000000000000000, -0.000000000000000000, -1.000000000000000000 ) ) ;
#1420 = PRESENTATION_LAYER_ASSIGNMENT (  '', '', ( #438 ) ) ;
#1421 = DIRECTION ( 'NONE',  ( 0.000000000000000000, 0.000000000000000000, 1.000000000000000000 ) ) ;
#1422 = ADVANCED_FACE ( 'NONE', ( #1497 ), #1708, .F. ) ;
#1423 = ORIENTED_EDGE ( 'NONE', *, *, #295, .F. ) ;
#1424 = ORIENTED_EDGE ( 'NONE', *, *, #1987, .T. ) ;
#1425 = CARTESIAN_POINT ( 'NONE',  ( 45.00000000000000000, 50.00000000000000000, 11.99999999999999645 ) ) ;
#1426 = SHAPE_DEFINITION_REPRESENTATION ( #1977, #107 ) ;
#1427 = ORIENTED_EDGE ( 'NONE', *, *, #907, .F. ) ;
#1428 = LINE ( 'NONE', #3027, #754 ) ;
#1429 = DIRECTION ( 'NONE',  ( 0.000000000000000000, 0.000000000000000000, 1.000000000000000000 ) ) ;
#1430 = DIRECTION ( 'NONE',  ( 0.000000000000000000, 0.000000000000000000, 1.000000000000000000 ) ) ;
#1431 = EDGE_CURVE ( 'NONE', #2174, #3236, #3284, .T. ) ;
#1432 = ORIENTED_EDGE ( 'NONE', *, *, #2774, .F. ) ;
#1433 = CARTESIAN_POINT ( 'NONE',  ( -54.99999999999995026, 130.0000000000000000, -4.999999999999997335 ) ) ;
#1434 = DIRECTION ( 'NONE',  ( 1.000000000000000000, 0.000000000000000000, 0.000000000000000000 ) ) ;
#1435 = ORIENTED_EDGE ( 'NONE', *, *, #3327, .F. ) ;
#1436 = CARTESIAN_POINT ( 'NONE',  ( 0.000000000000000000, -0.8865213383406730374, -1.535499999999999421 ) ) ;
#1437 = CARTESIAN_POINT ( 'NONE',  ( 0.000000000000000000, 0.000000000000000000, 83.99999999999998579 ) ) ;
#1438 = EDGE_LOOP ( 'NONE', ( #2817, #733, #2600, #2268 ) ) ;
#1439 = CARTESIAN_POINT ( 'NONE',  ( -44.99999999999999289, 50.00000000000000000, 12.00000000000000711 ) ) ;
#1440 = FILL_AREA_STYLE ('',( #404 ) ) ;
#1441 = DIRECTION ( 'NONE',  ( -1.000000000000000000, -0.000000000000000000, -0.000000000000000000 ) ) ;
#1442 = CARTESIAN_POINT ( 'NONE',  ( -44.99999999999999289, 52.00000000000000711, 10.00000000000000533 ) ) ;
#1443 = FILL_AREA_STYLE ('',( #1957 ) ) ;
#1444 = ADVANCED_FACE ( 'NONE', ( #3020 ), #677, .F. ) ;
#1445 = CARTESIAN_POINT ( 'NONE',  ( 55.00000000000004974, 130.0000000000000000, 5.000000000000004441 ) ) ;
#1446 = CARTESIAN_POINT ( 'NONE',  ( 2.000000000000000000, -0.8865213383406694847, 1.535500000000001419 ) ) ;
#1447 =( LENGTH_UNIT ( ) NAMED_UNIT ( * ) SI_UNIT ( .MILLI., .METRE. ) );
#1448 = EDGE_CURVE ( 'NONE', #2342, #2464, #1467, .T. ) ;
#1449 = ORIENTED_EDGE ( 'NONE', *, *, #1779, .F. ) ;
#1450 = LINE ( 'NONE', #1487, #2443 ) ;
#1451 = DIRECTION ( 'NONE',  ( -1.000000000000000000, 0.000000000000000000, 0.000000000000000000 ) ) ;
#1452 = EDGE_LOOP ( 'NONE', ( #1334, #2743, #2444, #3065 ) ) ;
#1453 = LINE ( 'NONE', #618, #1026 ) ;
#1454 = AXIS2_PLACEMENT_3D ( 'NONE', #2983, #185, #1483 ) ;
#1455 = VECTOR ( 'NONE', #267, 1000.000000000000000 ) ;
#1456 = ADVANCED_FACE ( 'NONE', ( #991 ), #1356, .F. ) ;
#1457 = CIRCLE ( 'NONE', #1032, 1.535500000000000087 ) ;
#1458 = CARTESIAN_POINT ( 'NONE',  ( -31.74999999999995737, 0.000000000000000000, 0.000000000000000000 ) ) ;
#1459 = PRODUCT_DEFINITION_SHAPE ( 'NONE', 'NONE',  #66 ) ;
#1460 = DIRECTION ( 'NONE',  ( 6.938893903907229364E-16, 0.000000000000000000, -1.000000000000000000 ) ) ;
#1461 = AXIS2_PLACEMENT_3D ( 'NONE', #2499, #163, #244 ) ;
#1462 = DIRECTION ( 'NONE',  ( 0.000000000000000000, 0.000000000000000000, 1.000000000000000000 ) ) ;
#1463 =( REPRESENTATION_RELATIONSHIP ('NONE','NONE', #3165, #714 ) REPRESENTATION_RELATIONSHIP_WITH_TRANSFORMATION ( #2839 )SHAPE_REPRESENTATION_RELATIONSHIP( ) );
#1464 = VECTOR ( 'NONE', #2850, 1000.000000000000000 ) ;
#1465 = AXIS2_PLACEMENT_3D ( 'NONE', #395, #1219, #2795 ) ;
#1466 = DIRECTION ( 'NONE',  ( -1.000000000000000000, -0.000000000000000000, -0.000000000000000000 ) ) ;
#1467 = LINE ( 'NONE', #3337, #2121 ) ;
#1468 = STYLED_ITEM ( 'NONE', ( #882 ), #930 ) ;
#1469 = ORIENTED_EDGE ( 'NONE', *, *, #3129, .T. ) ;
#1470 = COLOUR_RGB ( '',0.8941176470588234615, 0.8941176470588234615, 0.8941176470588234615 ) ;
#1471 = FACE_OUTER_BOUND ( 'NONE', #1724, .T. ) ;
#1472 = UNCERTAINTY_MEASURE_WITH_UNIT (LENGTH_MEASURE( 1.000000000000000082E-05 ), #1056, 'distance_accuracy_value', 'NONE');
#1473 = ADVANCED_FACE ( 'NONE', ( #3128 ), #644, .T. ) ;
#1474 = APPLICATION_PROTOCOL_DEFINITION ( 'draft international standard', 'automotive_design', 1998, #1502 ) ;
#1475 = ORIENTED_EDGE ( 'NONE', *, *, #3129, .F. ) ;
#1476 = AXIS2_PLACEMENT_3D ( 'NONE', #1650, #1115, #3159 ) ;
#1477 = DIRECTION ( 'NONE',  ( 0.000000000000000000, 1.000000000000000000, -1.345283343056720273E-15 ) ) ;
#1478 = ORIENTED_EDGE ( 'NONE', *, *, #1551, .F. ) ;
#1479 = CARTESIAN_POINT ( 'NONE',  ( -74.99999999999998579, 0.000000000000000000, -50.00000000000000000 ) ) ;
#1480 = DIRECTION ( 'NONE',  ( 0.000000000000000000, 0.000000000000000000, 1.000000000000000000 ) ) ;
#1481 = EDGE_CURVE ( 'NONE', #499, #3078, #1093, .T. ) ;
#1482 = CARTESIAN_POINT ( 'NONE',  ( 66.99999999999997158, 0.000000000000000000, 44.49999999999999289 ) ) ;
#1483 = DIRECTION ( 'NONE',  ( 0.000000000000000000, 0.000000000000000000, 1.000000000000000000 ) ) ;
#1484 = CARTESIAN_POINT ( 'NONE',  ( -40.00000000000000000, 52.00000000000000711, -4.999999999999995559 ) ) ;
#1485 = CARTESIAN_POINT ( 'NONE',  ( -66.99999999999997158, -5.000000000000000000, 41.99999999999999289 ) ) ;
#1486 = ORIENTED_EDGE ( 'NONE', *, *, #1804, .T. ) ;
#1487 = CARTESIAN_POINT ( 'NONE',  ( 66.99999999999997158, -5.000000000000000000, 44.49999999999999289 ) ) ;
#1488 = ORIENTED_EDGE ( 'NONE', *, *, #2475, .T. ) ;
#1489 = EDGE_CURVE ( 'NONE', #3137, #2129, #509, .T. ) ;
#1490 = FACE_OUTER_BOUND ( 'NONE', #2954, .T. ) ;
#1491 = ORIENTED_EDGE ( 'NONE', *, *, #3017, .F. ) ;
#1492 = EDGE_CURVE ( 'NONE', #331, #22, #2340, .T. ) ;
#1493 = DIRECTION ( 'NONE',  ( -0.000000000000000000, 1.000000000000000000, -0.000000000000000000 ) ) ;
#1494 = PRESENTATION_STYLE_ASSIGNMENT (( #456 ) ) ;
#1495 = DIRECTION ( 'NONE',  ( 1.000000000000000000, -0.000000000000000000, 0.000000000000000000 ) ) ;
#1496 = DIRECTION ( 'NONE',  ( -1.000000000000000000, -0.000000000000000000, -0.000000000000000000 ) ) ;
#1497 = FACE_OUTER_BOUND ( 'NONE', #1401, .T. ) ;
#1498 = EDGE_LOOP ( 'NONE', ( #71, #2016, #2376, #1158 ) ) ;
#1499 = ADVANCED_FACE ( 'NONE', ( #2862 ), #771, .T. ) ;
#1500 = ORIENTED_EDGE ( 'NONE', *, *, #1764, .T. ) ;
#1501 = CARTESIAN_POINT ( 'NONE',  ( -54.99999999999995026, 120.0000000000000142, -4.999999999999997335 ) ) ;
#1502 = APPLICATION_CONTEXT ( 'automotive_design' ) ;
#1503 = ORIENTED_EDGE ( 'NONE', *, *, #3252, .T. ) ;
#1504 = CARTESIAN_POINT ( 'NONE',  ( -66.99999999999997158, -5.000000000000000000, -41.99999999999999289 ) ) ;
#1505 = ORIENTED_EDGE ( 'NONE', *, *, #1448, .T. ) ;
#1506 = ADVANCED_BREP_SHAPE_REPRESENTATION ( '', ( #2945, #3111 ), #2889 ) ;
#1507 = AXIS2_PLACEMENT_3D ( 'NONE', #3336, #1295, #2333 ) ;
#1508 = CARTESIAN_POINT ( 'NONE',  ( -66.99999999999997158, -6.000000000000000000, 35.99999999999999289 ) ) ;
#1509 = CARTESIAN_POINT ( 'NONE',  ( 75.00000000000000000, 50.00000000000000000, -50.00000000000000000 ) ) ;
#1510 = EDGE_CURVE ( 'NONE', #1277, #3026, #758, .T. ) ;
#1511 = AXIS2_PLACEMENT_3D ( 'NONE', #1442, #688, #1480 ) ;
#1512 = AXIS2_PLACEMENT_3D ( 'NONE', #605, #1116, #1886 ) ;
#1513 = CARTESIAN_POINT ( 'NONE',  ( -66.99999999999997158, 0.000000000000000000, -41.99999999999999289 ) ) ;
#1514 = CARTESIAN_POINT ( 'NONE',  ( -74.99999999999998579, 0.000000000000000000, -50.00000000000000000 ) ) ;
#1515 = AXIS2_PLACEMENT_3D ( 'NONE', #557, #1585, #3230 ) ;
#1516 = CARTESIAN_POINT ( 'NONE',  ( 0.1999999999999987899, 0.000000000000000000, 0.000000000000000000 ) ) ;
#1517 = TOROIDAL_SURFACE ( 'NONE', #3158, 3.299999999999999822, 0.2000000000000000111 ) ;
#1518 = FACE_OUTER_BOUND ( 'NONE', #2894, .T. ) ;
#1519 = AXIS2_PLACEMENT_3D ( 'NONE', #2919, #2709, #2204 ) ;
#1520 = VECTOR ( 'NONE', #3073, 1000.000000000000000 ) ;
#1521 = ORIENTED_EDGE ( 'NONE', *, *, #603, .T. ) ;
#1522 = EDGE_LOOP ( 'NONE', ( #632, #2728, #1292, #2496 ) ) ;
#1523 = DIRECTION ( 'NONE',  ( 0.000000000000000000, -0.5000000000000011102, -0.8660254037844379305 ) ) ;
#1524 = VECTOR ( 'NONE', #1220, 999.9999999999998863 ) ;
#1525 = CIRCLE ( 'NONE', #1956, 7.500000000000000000 ) ;
#1526 = PRODUCT_DEFINITION ( 'UNKNOWN', '', #2020, #3077 ) ;
#1527 = ITEM_DEFINED_TRANSFORMATION ( 'NONE', 'NONE', #2621,  #3111 ) ;
#1528 = AXIS2_PLACEMENT_3D ( 'NONE', #2778, #3031, #2008 ) ;
#1529 = EDGE_LOOP ( 'NONE', ( #1381, #2933, #142, #1174 ) ) ;
#1530 = DIRECTION ( 'NONE',  ( -1.000000000000000000, 0.000000000000000000, 6.938893903907232322E-16 ) ) ;
#1531 = VERTEX_POINT ( 'NONE', #1062 ) ;
#1532 = SURFACE_STYLE_FILL_AREA ( #2059 ) ;
#1533 = DIRECTION ( 'NONE',  ( -0.000000000000000000, 1.000000000000000000, -0.000000000000000000 ) ) ;
#1534 = FACE_OUTER_BOUND ( 'NONE', #1814, .T. ) ;
#1535 = EDGE_CURVE ( 'NONE', #468, #2976, #1198, .T. ) ;
#1536 = DIRECTION ( 'NONE',  ( 0.000000000000000000, -1.000000000000000000, 0.000000000000000000 ) ) ;
#1537 = CARTESIAN_POINT ( 'NONE',  ( 2.000000000000000000, -0.8865213383406730374, -1.535499999999999421 ) ) ;
#1538 = VERTEX_POINT ( 'NONE', #495 ) ;
#1539 = VERTEX_POINT ( 'NONE', #1821 ) ;
#1540 = DIRECTION ( 'NONE',  ( 1.000000000000000000, -0.000000000000000000, 6.938893903907229364E-16 ) ) ;
#1541 = UNCERTAINTY_MEASURE_WITH_UNIT (LENGTH_MEASURE( 1.000000000000000082E-05 ), #2715, 'distance_accuracy_value', 'NONE');
#1542 = ORIENTED_EDGE ( 'NONE', *, *, #2186, .T. ) ;
#1543 = FACE_OUTER_BOUND ( 'NONE', #1674, .T. ) ;
#1544 = SHAPE_REPRESENTATION_RELATIONSHIP ( 'NONE' , 'NONE' ,  #936, #516 ) ;
#1545 = ORIENTED_EDGE ( 'NONE', *, *, #1804, .F. ) ;
#1546 = DIRECTION ( 'NONE',  ( 1.000000000000000000, 0.000000000000000000, 0.000000000000000000 ) ) ;
#1547 = CARTESIAN_POINT ( 'NONE',  ( -49.99999999999999289, 120.0000000000000142, -4.999999999999995559 ) ) ;
#1548 = PLANE ( 'NONE',  #870 ) ;
#1549 = DIRECTION ( 'NONE',  ( 0.000000000000000000, 0.000000000000000000, 1.000000000000000000 ) ) ;
#1550 = CARTESIAN_POINT ( 'NONE',  ( -40.00000000000000000, 52.00000000000000711, -4.999999999999996447 ) ) ;
#1551 = EDGE_CURVE ( 'NONE', #719, #35, #523, .T. ) ;
#1552 =( NAMED_UNIT ( * ) SI_UNIT ( $, .STERADIAN. ) SOLID_ANGLE_UNIT ( ) );
#1553 = ORIENTED_EDGE ( 'NONE', *, *, #1068, .F. ) ;
#1554 = VERTEX_POINT ( 'NONE', #1807 ) ;
#1555 = DIRECTION ( 'NONE',  ( -0.000000000000000000, 1.000000000000000000, -0.000000000000000000 ) ) ;
#1556 = EDGE_CURVE ( 'NONE', #1570, #1763, #158, .T. ) ;
#1557 = CONTEXT_DEPENDENT_SHAPE_REPRESENTATION ( #46, #785 ) ;
#1558 = EDGE_LOOP ( 'NONE', ( #1692, #264, #2437 ) ) ;
#1559 = FACE_BOUND ( 'NONE', #2192, .T. ) ;
#1560 =( LENGTH_UNIT ( ) NAMED_UNIT ( * ) SI_UNIT ( .MILLI., .METRE. ) );
#1561 = EDGE_LOOP ( 'NONE', ( #2255, #1811 ) ) ;
#1562 = CARTESIAN_POINT ( 'NONE',  ( 0.000000000000000000, 0.000000000000000000, 3.299999999999999822 ) ) ;
#1563 = PRESENTATION_STYLE_ASSIGNMENT (( #3349 ) ) ;
#1564 = EDGE_CURVE ( 'NONE', #223, #2834, #2880, .T. ) ;
#1565 = CARTESIAN_POINT ( 'NONE',  ( 0.000000000000000000, 52.00000000000000711, 0.000000000000000000 ) ) ;
#1566 = CARTESIAN_POINT ( 'NONE',  ( -49.99999999999999289, 120.0000000000000142, -4.999999999999995559 ) ) ;
#1567 = DIRECTION ( 'NONE',  ( 1.000000000000000000, 0.000000000000000000, 0.000000000000000000 ) ) ;
#1568 = VECTOR ( 'NONE', #182, 1000.000000000000227 ) ;
#1569 = CARTESIAN_POINT ( 'NONE',  ( -40.00000000000000000, 52.00000000000000711, -14.99999999999999645 ) ) ;
#1570 = VERTEX_POINT ( 'NONE', #1282 ) ;
#1571 = CIRCLE ( 'NONE', #3269, 2.000000000000001776 ) ;
#1572 = AXIS2_PLACEMENT_3D ( 'NONE', #2156, #3225, #878 ) ;
#1573 = EDGE_LOOP ( 'NONE', ( #2660, #278, #1578, #1896 ) ) ;
#1574 = DIRECTION ( 'NONE',  ( 6.938893903907229364E-16, 0.000000000000000000, -1.000000000000000000 ) ) ;
#1575 = CIRCLE ( 'NONE', #2713, 6.000000000000005329 ) ;
#1576 = CONICAL_SURFACE ( 'NONE', #2554, 2.000000000000001776, 1.029744258676657642 ) ;
#1577 = PRODUCT ( 'switch^MAS-192', 'switch^MAS-192', '', ( #3242 ) ) ;
#1578 = ORIENTED_EDGE ( 'NONE', *, *, #3063, .T. ) ;
#1579 = AXIS2_PLACEMENT_3D ( 'NONE', #1963, #2758, #665 ) ;
#1580 = CIRCLE ( 'NONE', #2544, 2.000000000000001776 ) ;
#1581 = ADVANCED_FACE ( 'NONE', ( #2559 ), #1589, .F. ) ;
#1582 = DIRECTION ( 'NONE',  ( 0.000000000000000000, -1.000000000000000000, 9.783878858594328898E-16 ) ) ;
#1583 = SURFACE_SIDE_STYLE ('',( #1239 ) ) ;
#1584 = ORIENTED_EDGE ( 'NONE', *, *, #2521, .T. ) ;
#1585 = DIRECTION ( 'NONE',  ( -0.000000000000000000, 1.000000000000000000, -0.000000000000000000 ) ) ;
#1586 = DIRECTION ( 'NONE',  ( 0.000000000000000000, -1.000000000000000000, -0.000000000000000000 ) ) ;
#1587 = PRODUCT_DEFINITION_FORMATION_WITH_SPECIFIED_SOURCE ( 'ANY', '', #1790, .NOT_KNOWN. ) ;
#1588 = DIRECTION ( 'NONE',  ( 0.000000000000000000, 0.000000000000000000, 1.000000000000000000 ) ) ;
#1589 = CYLINDRICAL_SURFACE ( 'NONE', #3048, 2.000000000000001776 ) ;
#1590 = CARTESIAN_POINT ( 'NONE',  ( -66.99999999999997158, -8.000000000000000000, 41.99999999999999289 ) ) ;
#1591 = EDGE_LOOP ( 'NONE', ( #2711, #1432 ) ) ;
#1592 = EDGE_LOOP ( 'NONE', ( #2893, #3324 ) ) ;
#1593 = CARTESIAN_POINT ( 'NONE',  ( 0.1999999999999987899, 0.000000000000000000, 0.000000000000000000 ) ) ;
#1594 = ORIENTED_EDGE ( 'NONE', *, *, #2514, .F. ) ;
#1595 = CYLINDRICAL_SURFACE ( 'NONE', #49, 2.149999999999999023 ) ;
#1596 = EDGE_CURVE ( 'NONE', #361, #608, #2608, .T. ) ;
#1597 = PRESENTATION_STYLE_ASSIGNMENT (( #1647 ) ) ;
#1598 = ORIENTED_EDGE ( 'NONE', *, *, #2097, .F. ) ;
#1599 = DIRECTION ( 'NONE',  ( -0.000000000000000000, 1.000000000000000000, -0.000000000000000000 ) ) ;
#1600 = EDGE_CURVE ( 'NONE', #361, #699, #1022, .T. ) ;
#1601 = DIRECTION ( 'NONE',  ( 0.000000000000000000, 0.5150380749100514910, 0.8571673007021138879 ) ) ;
#1602 = DIRECTION ( 'NONE',  ( 0.000000000000000000, 0.000000000000000000, 1.000000000000000000 ) ) ;
#1603 = CARTESIAN_POINT ( 'NONE',  ( -66.99999999999997158, -8.000000000000000000, 41.99999999999999289 ) ) ;
#1604 = ORIENTED_EDGE ( 'NONE', *, *, #2037, .F. ) ;
#1605 = VERTEX_POINT ( 'NONE', #19 ) ;
#1606 = CARTESIAN_POINT ( 'NONE',  ( -50.00000000000000000, 120.0000000000000142, 5.000000000000004441 ) ) ;
#1607 = EDGE_CURVE ( 'NONE', #2174, #1994, #2628, .T. ) ;
#1608 = ORIENTED_EDGE ( 'NONE', *, *, #352, .F. ) ;
#1609 = CARTESIAN_POINT ( 'NONE',  ( 44.99999999999999289, 45.00000000000000711, -10.00000000000000533 ) ) ;
#1610 = DIRECTION ( 'NONE',  ( 0.000000000000000000, 0.000000000000000000, 1.000000000000000000 ) ) ;
#1611 = ORIENTED_EDGE ( 'NONE', *, *, #2350, .T. ) ;
#1612 = FACE_OUTER_BOUND ( 'NONE', #2099, .T. ) ;
#1613 =( NAMED_UNIT ( * ) PLANE_ANGLE_UNIT ( ) SI_UNIT ( $, .RADIAN. ) );
#1614 = LINE ( 'NONE', #2162, #1729 ) ;
#1615 = CARTESIAN_POINT ( 'NONE',  ( 0.000000000000000000, 25.00000000000000000, 47.00000000000000000 ) ) ;
#1616 = ADVANCED_FACE ( 'NONE', ( #3086 ), #2849, .F. ) ;
#1617 = CARTESIAN_POINT ( 'NONE',  ( 4.000000000000003553, 0.000000000000000000, 0.000000000000000000 ) ) ;
#1618 = EDGE_LOOP ( 'NONE', ( #4, #2118, #226, #2844 ) ) ;
#1619 = EDGE_LOOP ( 'NONE', ( #2362, #3177, #1371, #1140 ) ) ;
#1620 = DIRECTION ( 'NONE',  ( 0.000000000000000000, 0.5150380749100514910, 0.8571673007021138879 ) ) ;
#1621 = CARTESIAN_POINT ( 'NONE',  ( -40.00000000000000000, 120.0000000000000142, -4.999999999999995559 ) ) ;
#1622 = VECTOR ( 'NONE', #622, 1000.000000000000000 ) ;
#1623 = ORIENTED_EDGE ( 'NONE', *, *, #794, .F. ) ;
#1624 = DIRECTION ( 'NONE',  ( -0.000000000000000000, -1.000000000000000000, -0.000000000000000000 ) ) ;
#1625 = VECTOR ( 'NONE', #2256, 1000.000000000000000 ) ;
#1626 = EDGE_CURVE ( 'NONE', #3026, #1277, #980, .T. ) ;
#1627 =( NAMED_UNIT ( * ) PLANE_ANGLE_UNIT ( ) SI_UNIT ( $, .RADIAN. ) );
#1628 = AXIS2_PLACEMENT_3D ( 'NONE', #3239, #2693, #1695 ) ;
#1629 = VECTOR ( 'NONE', #1567, 1000.000000000000000 ) ;
#1630 = ORIENTED_EDGE ( 'NONE', *, *, #2240, .F. ) ;
#1631 = CARTESIAN_POINT ( 'NONE',  ( 2.886521338340684917, 0.000000000000000000, 0.000000000000000000 ) ) ;
#1632 =( GEOMETRIC_REPRESENTATION_CONTEXT ( 3 ) GLOBAL_UNCERTAINTY_ASSIGNED_CONTEXT ( ( #2944 ) ) GLOBAL_UNIT_ASSIGNED_CONTEXT ( ( #447, #3338, #524 ) ) REPRESENTATION_CONTEXT ( 'NONE', 'WORKASPACE' ) );
#1633 =( LENGTH_UNIT ( ) NAMED_UNIT ( * ) SI_UNIT ( .MILLI., .METRE. ) );
#1634 = COLOUR_RGB ( '',0.8941176470588234615, 0.8941176470588234615, 0.8941176470588234615 ) ;
#1635 = DIRECTION ( 'NONE',  ( 0.000000000000000000, 0.000000000000000000, 1.000000000000000000 ) ) ;
#1636 = DIRECTION ( 'NONE',  ( 1.000000000000000000, 0.000000000000000000, 0.000000000000000000 ) ) ;
#1637 = DIRECTION ( 'NONE',  ( 0.000000000000000000, 0.000000000000000000, 1.000000000000000000 ) ) ;
#1638 = ADVANCED_FACE ( 'NONE', ( #572 ), #303, .F. ) ;
#1639 = ORIENTED_EDGE ( 'NONE', *, *, #1535, .T. ) ;
#1640 = ORIENTED_EDGE ( 'NONE', *, *, #248, .T. ) ;
#1641 = AXIS2_PLACEMENT_3D ( 'NONE', #2764, #1223, #2254 ) ;
#1642 = FACE_BOUND ( 'NONE', #1265, .T. ) ;
#1643 = DIRECTION ( 'NONE',  ( 1.387778780781445676E-16, 0.000000000000000000, -1.000000000000000000 ) ) ;
#1644 = EDGE_CURVE ( 'NONE', #2597, #3240, #321, .T. ) ;
#1645 = EDGE_LOOP ( 'NONE', ( #667, #2491, #1298, #1064 ) ) ;
#1646 = LINE ( 'NONE', #2175, #2002 ) ;
#1647 = SURFACE_STYLE_USAGE ( .BOTH. , #2426 ) ;
#1648 = ORIENTED_EDGE ( 'NONE', *, *, #1448, .F. ) ;
#1649 = CARTESIAN_POINT ( 'NONE',  ( -40.00000000000000000, 117.0000000000000000, -4.999999999999995559 ) ) ;
#1650 = CARTESIAN_POINT ( 'NONE',  ( 0.000000000000000000, 0.000000000000000000, 0.000000000000000000 ) ) ;
#1651 = EDGE_CURVE ( 'NONE', #1297, #489, #2449, .T. ) ;
#1652 = CARTESIAN_POINT ( 'NONE',  ( 45.00000000000000000, 50.00000000000000000, 9.999999999999994671 ) ) ;
#1653 = CARTESIAN_POINT ( 'NONE',  ( 44.99999999999999289, 45.00000000000000711, -8.000000000000003553 ) ) ;
#1654 = CARTESIAN_POINT ( 'NONE',  ( -45.00000000000000000, 45.00000000000000711, -11.99999999999999645 ) ) ;
#1655 = ORIENTED_EDGE ( 'NONE', *, *, #1661, .T. ) ;
#1656 = ORIENTED_EDGE ( 'NONE', *, *, #868, .F. ) ;
#1657 = FACE_OUTER_BOUND ( 'NONE', #1862, .T. ) ;
#1658 = CARTESIAN_POINT ( 'NONE',  ( -54.99999999999995026, 130.0000000000000000, -4.999999999999997335 ) ) ;
#1659 = ORIENTED_EDGE ( 'NONE', *, *, #2417, .T. ) ;
#1660 = CARTESIAN_POINT ( 'NONE',  ( -40.00000000000000000, 120.0000000000000142, 5.000000000000004441 ) ) ;
#1661 = EDGE_CURVE ( 'NONE', #1274, #2252, #33, .T. ) ;
#1662 = CARTESIAN_POINT ( 'NONE',  ( 0.000000000000000000, 0.000000000000000000, 0.000000000000000000 ) ) ;
#1663 = EDGE_LOOP ( 'NONE', ( #1890, #465, #538, #1323 ) ) ;
#1664 = CARTESIAN_POINT ( 'NONE',  ( 2.000000000000000000, 1.773042676681340524, -2.059984127722458425E-15 ) ) ;
#1665 = CARTESIAN_POINT ( 'NONE',  ( -31.74999999999995737, 0.000000000000000000, 2.000000000000000888 ) ) ;
#1666 = CARTESIAN_POINT ( 'NONE',  ( 55.00000000000000000, 130.0000000000000000, -5.000000000000000000 ) ) ;
#1667 = EDGE_CURVE ( 'NONE', #824, #113, #82, .T. ) ;
#1668 = DIRECTION ( 'NONE',  ( 1.000000000000000000, 0.000000000000000000, -0.000000000000000000 ) ) ;
#1669 = VECTOR ( 'NONE', #2214, 1000.000000000000000 ) ;
#1670 = ORIENTED_EDGE ( 'NONE', *, *, #205, .F. ) ;
#1671 = EDGE_LOOP ( 'NONE', ( #1082, #2782, #293 ) ) ;
#1672 = DIRECTION ( 'NONE',  ( -0.000000000000000000, 1.000000000000000000, 1.224646799147353207E-16 ) ) ;
#1673 = LINE ( 'NONE', #890, #1952 ) ;
#1674 = EDGE_LOOP ( 'NONE', ( #2406, #735, #679, #238 ) ) ;
#1675 = DIRECTION ( 'NONE',  ( -1.000000000000000000, -0.000000000000000000, -0.000000000000000000 ) ) ;
#1676 =( GEOMETRIC_REPRESENTATION_CONTEXT ( 3 ) GLOBAL_UNCERTAINTY_ASSIGNED_CONTEXT ( ( #581 ) ) GLOBAL_UNIT_ASSIGNED_CONTEXT ( ( #795, #2859, #3124 ) ) REPRESENTATION_CONTEXT ( 'NONE', 'WORKASPACE' ) );
#1677 = DIRECTION ( 'NONE',  ( 6.123233995736766036E-17, -1.000000000000000000, 0.000000000000000000 ) ) ;
#1678 = APPLICATION_CONTEXT ( 'automotive_design' ) ;
#1679 = ORIENTED_EDGE ( 'NONE', *, *, #16, .T. ) ;
#1680 = ADVANCED_FACE ( 'NONE', ( #1117 ), #50, .F. ) ;
#1681 = CIRCLE ( 'NONE', #1894, 2.149999999999999023 ) ;
#1682 = AXIS2_PLACEMENT_3D ( 'NONE', #23, #1540, #1574 ) ;
#1683 = DIRECTION ( 'NONE',  ( -0.000000000000000000, 1.000000000000000000, -0.000000000000000000 ) ) ;
#1684 = VECTOR ( 'NONE', #517, 1000.000000000000000 ) ;
#1685 = VECTOR ( 'NONE', #2140, 1000.000000000000000 ) ;
#1686 = CARTESIAN_POINT ( 'NONE',  ( -7.250000000000000000, 25.00000000000000000, 47.00000000000000000 ) ) ;
#1687 = AXIS2_PLACEMENT_3D ( 'NONE', #2459, #99, #2967 ) ;
#1688 = DIRECTION ( 'NONE',  ( 0.000000000000000000, 1.000000000000000000, -1.224646799147353207E-16 ) ) ;
#1689 = CIRCLE ( 'NONE', #2010, 3.299999999999999822 ) ;
#1690 = PLANE ( 'NONE',  #928 ) ;
#1691 = AXIS2_PLACEMENT_3D ( 'NONE', #1246, #939, #3018 ) ;
#1692 = ORIENTED_EDGE ( 'NONE', *, *, #310, .F. ) ;
#1693 = CARTESIAN_POINT ( 'NONE',  ( -39.00000000000000000, 117.0000000000000000, 5.000000000000004441 ) ) ;
#1694 = LINE ( 'NONE', #956, #432 ) ;
#1695 = DIRECTION ( 'NONE',  ( 0.000000000000000000, 0.000000000000000000, -1.000000000000000000 ) ) ;
#1696 = VERTEX_POINT ( 'NONE', #606 ) ;
#1697 = CARTESIAN_POINT ( 'NONE',  ( -39.99999999999999289, 52.00000000000000711, 15.00000000000000178 ) ) ;
#1698 = DIRECTION ( 'NONE',  ( 0.000000000000000000, 0.000000000000000000, 1.000000000000000000 ) ) ;
#1699 = ORIENTED_EDGE ( 'NONE', *, *, #392, .T. ) ;
#1700 = CARTESIAN_POINT ( 'NONE',  ( -49.99999999999999289, 52.00000000000000711, -14.99999999999999645 ) ) ;
#1701 = EDGE_CURVE ( 'NONE', #2306, #38, #1887, .T. ) ;
#1702 =( NAMED_UNIT ( * ) SI_UNIT ( $, .STERADIAN. ) SOLID_ANGLE_UNIT ( ) );
#1703 = CARTESIAN_POINT ( 'NONE',  ( -66.99999999999997158, 0.000000000000000000, 39.50000000000000000 ) ) ;
#1704 = CARTESIAN_POINT ( 'NONE',  ( 66.99999999999997158, -5.000000000000000000, -41.99999999999999289 ) ) ;
#1705 = EDGE_CURVE ( 'NONE', #2405, #2003, #2149, .T. ) ;
#1706 =( REPRESENTATION_RELATIONSHIP ('NONE','NONE', #3165, #1286 ) REPRESENTATION_RELATIONSHIP_WITH_TRANSFORMATION ( #3004 )SHAPE_REPRESENTATION_RELATIONSHIP( ) );
#1707 = DIRECTION ( 'NONE',  ( 1.000000000000000000, 0.000000000000000000, 0.000000000000000000 ) ) ;
#1708 = PLANE ( 'NONE',  #387 ) ;
#1709 = ORIENTED_EDGE ( 'NONE', *, *, #36, .F. ) ;
#1710 = DIRECTION ( 'NONE',  ( -0.000000000000000000, -1.000000000000000000, -0.000000000000000000 ) ) ;
#1711 = UNCERTAINTY_MEASURE_WITH_UNIT (LENGTH_MEASURE( 1.000000000000000082E-05 ), #3067, 'distance_accuracy_value', 'NONE');
#1712 = EDGE_CURVE ( 'NONE', #2643, #229, #2914, .T. ) ;
#1713 = APPLICATION_PROTOCOL_DEFINITION ( 'draft international standard', 'automotive_design', 1998, #738 ) ;
#1714 = EDGE_LOOP ( 'NONE', ( #780, #10, #1382, #3341 ) ) ;
#1715 = DIRECTION ( 'NONE',  ( 0.000000000000000000, 0.000000000000000000, -1.000000000000000000 ) ) ;
#1716 = APPLICATION_PROTOCOL_DEFINITION ( 'draft international standard', 'automotive_design', 1998, #3321 ) ;
#1717 = CYLINDRICAL_SURFACE ( 'NONE', #366, 3.500000000000000000 ) ;
#1718 = DIRECTION ( 'NONE',  ( -0.000000000000000000, -0.000000000000000000, 1.000000000000000000 ) ) ;
#1719 = SURFACE_SIDE_STYLE ('',( #2793 ) ) ;
#1720 = DIRECTION ( 'NONE',  ( 0.000000000000000000, 0.000000000000000000, 1.000000000000000000 ) ) ;
#1721 = EDGE_CURVE ( 'NONE', #2239, #2464, #2688, .T. ) ;
#1722 = DIRECTION ( 'NONE',  ( 0.000000000000000000, 0.000000000000000000, -1.000000000000000000 ) ) ;
#1723 = PLANE ( 'NONE',  #1579 ) ;
#1724 = EDGE_LOOP ( 'NONE', ( #208, #88 ) ) ;
#1725 = CYLINDRICAL_SURFACE ( 'NONE', #1249, 2.149999999999999023 ) ;
#1726 = EDGE_LOOP ( 'NONE', ( #203, #1025, #454, #2305 ) ) ;
#1727 = EDGE_CURVE ( 'NONE', #1875, #1319, #1580, .T. ) ;
#1728 = CARTESIAN_POINT ( 'NONE',  ( 0.000000000000000000, 1.773042676681340524, -2.059984127722458425E-15 ) ) ;
#1729 = VECTOR ( 'NONE', #31, 1000.000000000000114 ) ;
#1730 = PRESENTATION_STYLE_ASSIGNMENT (( #3246 ) ) ;
#1731 = CONICAL_SURFACE ( 'NONE', #3157, 2.000000000000001776, 1.029744258676657642 ) ;
#1732 = AXIS2_PLACEMENT_3D ( 'NONE', #1818, #2532, #2858 ) ;
#1733 = ORIENTED_EDGE ( 'NONE', *, *, #352, .T. ) ;
#1734 = DIRECTION ( 'NONE',  ( 1.000000000000000000, 0.000000000000000000, 0.000000000000000000 ) ) ;
#1735 = PLANE ( 'NONE',  #42 ) ;
#1736 = AXIS2_PLACEMENT_3D ( 'NONE', #1816, #1307, #1238 ) ;
#1737 = VECTOR ( 'NONE', #239, 1000.000000000000000 ) ;
#1738 = PRESENTATION_LAYER_ASSIGNMENT (  '', '', ( #2009 ) ) ;
#1739 = PLANE ( 'NONE',  #1454 ) ;
#1740 = CARTESIAN_POINT ( 'NONE',  ( 7.250000000000000000, 25.00000000000000000, 47.00000000000000000 ) ) ;
#1741 = VECTOR ( 'NONE', #148, 1000.000000000000000 ) ;
#1742 = EDGE_CURVE ( 'NONE', #2100, #880, #2674, .T. ) ;
#1743 = PRESENTATION_STYLE_ASSIGNMENT (( #3021 ) ) ;
#1744 = ORIENTED_EDGE ( 'NONE', *, *, #1206, .F. ) ;
#1745 = MECHANICAL_DESIGN_GEOMETRIC_PRESENTATION_REPRESENTATION (  '', ( #2235 ), #2722 ) ;
#1746 = CARTESIAN_POINT ( 'NONE',  ( 4.000000000000001776, 2.694222958124178486E-16, 2.200000000000001066 ) ) ;
#1747 = EDGE_CURVE ( 'NONE', #2320, #719, #1078, .T. ) ;
#1748 = PRODUCT_DEFINITION_FORMATION_WITH_SPECIFIED_SOURCE ( 'ANY', '', #455, .NOT_KNOWN. ) ;
#1749 = ORIENTED_EDGE ( 'NONE', *, *, #1411, .F. ) ;
#1750 = CARTESIAN_POINT ( 'NONE',  ( 45.00000000000000000, 43.79827876194489278, 9.999999999999994671 ) ) ;
#1751 = VERTEX_POINT ( 'NONE', #2416 ) ;
#1752 = DIRECTION ( 'NONE',  ( 0.000000000000000000, 0.000000000000000000, -1.000000000000000000 ) ) ;
#1753 = CARTESIAN_POINT ( 'NONE',  ( 2.000000000000000000, -1.773042676681341856, 2.276824562219559311E-15 ) ) ;
#1754 = ADVANCED_FACE ( 'NONE', ( #1131 ), #2164, .F. ) ;
#1755 = CARTESIAN_POINT ( 'NONE',  ( -7.500000000000000000, 25.00000000000000000, 50.00000000000000000 ) ) ;
#1756 = DIRECTION ( 'NONE',  ( 0.000000000000000000, 0.000000000000000000, 1.000000000000000000 ) ) ;
#1757 = CARTESIAN_POINT ( 'NONE',  ( 4.000000000000003553, 4.286263797015736595E-16, -3.500000000000000000 ) ) ;
#1758 = FILL_AREA_STYLE ('',( #3268 ) ) ;
#1759 = ORIENTED_EDGE ( 'NONE', *, *, #741, .F. ) ;
#1760 = ORIENTED_EDGE ( 'NONE', *, *, #503, .T. ) ;
#1761 = CARTESIAN_POINT ( 'NONE',  ( -40.00000000000000000, 120.0000000000000142, 5.000000000000004441 ) ) ;
#1762 = CONTEXT_DEPENDENT_SHAPE_REPRESENTATION ( #3257, #2366 ) ;
#1763 = VERTEX_POINT ( 'NONE', #1393 ) ;
#1764 = EDGE_CURVE ( 'NONE', #774, #561, #2432, .T. ) ;
#1765 = LINE ( 'NONE', #759, #1355 ) ;
#1766 = ORIENTED_EDGE ( 'NONE', *, *, #3357, .F. ) ;
#1767 = LINE ( 'NONE', #246, #1027 ) ;
#1768 = DIRECTION ( 'NONE',  ( -1.000000000000000000, -0.000000000000000000, -0.000000000000000000 ) ) ;
#1769 = LINE ( 'NONE', #2807, #816 ) ;
#1770 = DIRECTION ( 'NONE',  ( 0.000000000000000000, 0.000000000000000000, -1.000000000000000000 ) ) ;
#1771 = PRODUCT_RELATED_PRODUCT_CATEGORY ( 'part', '', ( #510 ) ) ;
#1772 = DIRECTION ( 'NONE',  ( 0.000000000000000000, 0.000000000000000000, -1.000000000000000000 ) ) ;
#1773 = DIRECTION ( 'NONE',  ( -0.000000000000000000, 1.000000000000000000, -0.000000000000000000 ) ) ;
#1774 = EDGE_LOOP ( 'NONE', ( #2358, #2785, #709 ) ) ;
#1775 = ORIENTED_EDGE ( 'NONE', *, *, #3153, .F. ) ;
#1776 = PLANE ( 'NONE',  #1090 ) ;
#1777 = ORIENTED_EDGE ( 'NONE', *, *, #825, .F. ) ;
#1778 = FACE_BOUND ( 'NONE', #651, .T. ) ;
#1779 = EDGE_CURVE ( 'NONE', #2115, #347, #2984, .T. ) ;
#1780 =( LENGTH_UNIT ( ) NAMED_UNIT ( * ) SI_UNIT ( .MILLI., .METRE. ) );
#1781 = ORIENTED_EDGE ( 'NONE', *, *, #630, .T. ) ;
#1782 = DIRECTION ( 'NONE',  ( 0.000000000000000000, 0.000000000000000000, 1.000000000000000000 ) ) ;
#1783 = FACE_OUTER_BOUND ( 'NONE', #2038, .T. ) ;
#1784 = MECHANICAL_DESIGN_GEOMETRIC_PRESENTATION_REPRESENTATION (  '', ( #2440 ), #1245 ) ;
#1785 = CARTESIAN_POINT ( 'NONE',  ( -50.00000000000000000, 117.0000000000000000, 6.000000000000004441 ) ) ;
#1786 = DIRECTION ( 'NONE',  ( 0.000000000000000000, 0.000000000000000000, 1.000000000000000000 ) ) ;
#1787 =( GEOMETRIC_REPRESENTATION_CONTEXT ( 3 ) GLOBAL_UNCERTAINTY_ASSIGNED_CONTEXT ( ( #760 ) ) GLOBAL_UNIT_ASSIGNED_CONTEXT ( ( #1279, #216, #2094 ) ) REPRESENTATION_CONTEXT ( 'NONE', 'WORKASPACE' ) );
#1788 = DIRECTION ( 'NONE',  ( 6.938893903907228378E-16, 0.000000000000000000, 1.000000000000000000 ) ) ;
#1789 = CIRCLE ( 'NONE', #3323, 1.535500000000000087 ) ;
#1790 = PRODUCT ( 'cross bar', 'cross bar', '', ( #669 ) ) ;
#1791 = SURFACE_STYLE_USAGE ( .BOTH. , #1008 ) ;
#1792 = VECTOR ( 'NONE', #1851, 1000.000000000000000 ) ;
#1793 = VECTOR ( 'NONE', #716, 1000.000000000000000 ) ;
#1794 = EDGE_LOOP ( 'NONE', ( #800, #1254, #958, #1475, #3271, #1984, #994, #326 ) ) ;
#1795 = ORIENTED_EDGE ( 'NONE', *, *, #2812, .F. ) ;
#1796 = CARTESIAN_POINT ( 'NONE',  ( -51.00000000000000000, 117.0000000000000000, -4.999999999999996447 ) ) ;
#1797 =( GEOMETRIC_REPRESENTATION_CONTEXT ( 3 ) GLOBAL_UNCERTAINTY_ASSIGNED_CONTEXT ( ( #2842 ) ) GLOBAL_UNIT_ASSIGNED_CONTEXT ( ( #747, #2575, #1552 ) ) REPRESENTATION_CONTEXT ( 'NONE', 'WORKASPACE' ) );
#1798 = VECTOR ( 'NONE', #1132, 1000.000000000000000 ) ;
#1799 = ORIENTED_EDGE ( 'NONE', *, *, #545, .F. ) ;
#1800 = DIRECTION ( 'NONE',  ( 0.000000000000000000, -0.000000000000000000, -1.000000000000000000 ) ) ;
#1801 = ORIENTED_EDGE ( 'NONE', *, *, #1852, .F. ) ;
#1802 =( GEOMETRIC_REPRESENTATION_CONTEXT ( 3 ) GLOBAL_UNCERTAINTY_ASSIGNED_CONTEXT ( ( #1541 ) ) GLOBAL_UNIT_ASSIGNED_CONTEXT ( ( #2715, #360, #631 ) ) REPRESENTATION_CONTEXT ( 'NONE', 'WORKASPACE' ) );
#1803 = DIRECTION ( 'NONE',  ( -0.000000000000000000, 1.000000000000000000, -0.000000000000000000 ) ) ;
#1804 = EDGE_CURVE ( 'NONE', #229, #1531, #1859, .T. ) ;
#1805 = CARTESIAN_POINT ( 'NONE',  ( 2.000000000000000000, 1.329782007511004727, -0.7677500000000018199 ) ) ;
#1806 = CARTESIAN_POINT ( 'NONE',  ( 2.000000000000000000, 1.773042676681340524, -2.059984127722458425E-15 ) ) ;
#1807 = CARTESIAN_POINT ( 'NONE',  ( 66.99999999999997158, -5.000000000000000000, -39.50000000000000000 ) ) ;
#1808 = EDGE_CURVE ( 'NONE', #1696, #1840, #1986, .T. ) ;
#1809 = CARTESIAN_POINT ( 'NONE',  ( -66.99999999999997158, -6.000000000000000000, 46.50000000000000711 ) ) ;
#1810 = ORIENTED_EDGE ( 'NONE', *, *, #1661, .F. ) ;
#1811 = ORIENTED_EDGE ( 'NONE', *, *, #1556, .F. ) ;
#1812 = CARTESIAN_POINT ( 'NONE',  ( -40.00000000000000000, 50.00000000000000000, -14.99999999999999645 ) ) ;
#1813 = ITEM_DEFINED_TRANSFORMATION ( 'NONE', 'NONE', #114,  #3111 ) ;
#1814 = EDGE_LOOP ( 'NONE', ( #562, #1344, #2718 ) ) ;
#1815 = ADVANCED_FACE ( 'NONE', ( #1973 ), #442, .F. ) ;
#1816 = CARTESIAN_POINT ( 'NONE',  ( 2.000000000000000000, -0.8865213383406694847, 1.535500000000001419 ) ) ;
#1817 = ORIENTED_EDGE ( 'NONE', *, *, #181, .T. ) ;
#1818 = CARTESIAN_POINT ( 'NONE',  ( 0.000000000000000000, 25.00000000000000000, 47.00000000000000000 ) ) ;
#1819 =( NAMED_UNIT ( * ) PLANE_ANGLE_UNIT ( ) SI_UNIT ( $, .RADIAN. ) );
#1820 = CARTESIAN_POINT ( 'NONE',  ( 66.99999999999997158, 0.000000000000000000, 39.50000000000000000 ) ) ;
#1821 = CARTESIAN_POINT ( 'NONE',  ( 45.00000000000000000, 50.00000000000000000, 7.999999999999992895 ) ) ;
#1822 = EDGE_CURVE ( 'NONE', #1843, #740, #2654, .T. ) ;
#1823 = EDGE_LOOP ( 'NONE', ( #950, #2865 ) ) ;
#1824 = ORIENTED_EDGE ( 'NONE', *, *, #2802, .F. ) ;
#1825 = DIRECTION ( 'NONE',  ( 6.938893903907229364E-16, 0.000000000000000000, -1.000000000000000000 ) ) ;
#1826 = EDGE_LOOP ( 'NONE', ( #2421, #551, #1010, #1500 ) ) ;
#1827 = CARTESIAN_POINT ( 'NONE',  ( -66.99999999999997158, -5.000000000000000000, 41.99999999999999289 ) ) ;
#1828 = CLOSED_SHELL ( 'NONE', ( #3339, #93, #362, #1680, #1456, #3315, #118, #1004, #633, #2560, #2361, #3191, #2610, #2538, #2953, #2707, #400, #2387, #1233, #425, #2453, #2428, #76, #1921, #2286, #953, #992, #492, #1499, #2631, #2731, #1929, #2201, #2088, #1218, #1581, #2161 ) ) ;
#1829 =( NAMED_UNIT ( * ) SI_UNIT ( $, .STERADIAN. ) SOLID_ANGLE_UNIT ( ) );
#1830 = PRODUCT_RELATED_PRODUCT_CATEGORY ( 'part', '', ( #235 ) ) ;
#1831 = ORIENTED_EDGE ( 'NONE', *, *, #886, .T. ) ;
#1832 = DIRECTION ( 'NONE',  ( 0.000000000000000000, 0.000000000000000000, 1.000000000000000000 ) ) ;
#1833 = LINE ( 'NONE', #1785, #2288 ) ;
#1834 = CIRCLE ( 'NONE', #2271, 2.000000000000000888 ) ;
#1835 = DIRECTION ( 'NONE',  ( 0.000000000000000000, -1.000000000000000000, 9.783878858594328898E-16 ) ) ;
#1836 = DIRECTION ( 'NONE',  ( 0.000000000000000000, 0.000000000000000000, 1.000000000000000000 ) ) ;
#1837 = PRESENTATION_LAYER_ASSIGNMENT (  '', '', ( #2220 ) ) ;
#1838 = VECTOR ( 'NONE', #145, 1000.000000000000000 ) ;
#1839 = LINE ( 'NONE', #3368, #2994 ) ;
#1840 = VERTEX_POINT ( 'NONE', #1229 ) ;
#1841 = VECTOR ( 'NONE', #3012, 1000.000000000000000 ) ;
#1842 = CIRCLE ( 'NONE', #98, 2.500000000000009326 ) ;
#1843 = VERTEX_POINT ( 'NONE', #2213 ) ;
#1844 = LINE ( 'NONE', #1796, #2336 ) ;
#1845 = EDGE_CURVE ( 'NONE', #2345, #2833, #2245, .T. ) ;
#1846 = AXIS2_PLACEMENT_3D ( 'NONE', #136, #475, #2537 ) ;
#1847 = AXIS2_PLACEMENT_3D ( 'NONE', #1516, #544, #2317 ) ;
#1848 = VERTEX_POINT ( 'NONE', #2005 ) ;
#1849 = COLOUR_RGB ( '',0.8941176470588234615, 0.8941176470588234615, 0.8941176470588234615 ) ;
#1850 = VECTOR ( 'NONE', #2641, 1000.000000000000000 ) ;
#1851 = DIRECTION ( 'NONE',  ( -0.000000000000000000, 1.000000000000000000, -0.000000000000000000 ) ) ;
#1852 = EDGE_CURVE ( 'NONE', #121, #3215, #3330, .T. ) ;
#1853 = AXIS2_PLACEMENT_3D ( 'NONE', #768, #2368, #2878 ) ;
#1854 =( NAMED_UNIT ( * ) PLANE_ANGLE_UNIT ( ) SI_UNIT ( $, .RADIAN. ) );
#1855 = ORIENTED_EDGE ( 'NONE', *, *, #137, .F. ) ;
#1856 = DIRECTION ( 'NONE',  ( 1.000000000000000000, 0.000000000000000000, 0.000000000000000000 ) ) ;
#1857 = APPLICATION_CONTEXT ( 'automotive_design' ) ;
#1858 = LINE ( 'NONE', #2640, #2931 ) ;
#1859 = LINE ( 'NONE', #2898, #1850 ) ;
#1860 = ADVANCED_FACE ( 'NONE', ( #2504 ), #1735, .T. ) ;
#1861 = CARTESIAN_POINT ( 'NONE',  ( -66.99999999999997158, -8.000000000000000000, 46.50000000000000711 ) ) ;
#1862 = EDGE_LOOP ( 'NONE', ( #2990, #2526, #1284, #692, #1545, #1424, #3319, #1817 ) ) ;
#1863 = ORIENTED_EDGE ( 'NONE', *, *, #2243, .T. ) ;
#1864 = PLANE ( 'NONE',  #811 ) ;
#1865 = EDGE_LOOP ( 'NONE', ( #1855, #2824 ) ) ;
#1866 = CARTESIAN_POINT ( 'NONE',  ( -39.99999999999999289, 50.00000000000000000, 15.00000000000000178 ) ) ;
#1867 = CARTESIAN_POINT ( 'NONE',  ( 0.000000000000000000, 0.000000000000000000, 0.000000000000000000 ) ) ;
#1868 = ORIENTED_EDGE ( 'NONE', *, *, #1288, .T. ) ;
#1869 = EDGE_CURVE ( 'NONE', #531, #2478, #2777, .T. ) ;
#1870 = DIRECTION ( 'NONE',  ( 0.000000000000000000, 0.000000000000000000, -1.000000000000000000 ) ) ;
#1871 = CARTESIAN_POINT ( 'NONE',  ( 0.000000000000000000, 0.000000000000000000, 0.000000000000000000 ) ) ;
#1872 = CARTESIAN_POINT ( 'NONE',  ( 10.00000000000000178, 0.000000000000000000, 0.000000000000000000 ) ) ;
#1873 = DIRECTION ( 'NONE',  ( 0.000000000000000000, 0.000000000000000000, 1.000000000000000000 ) ) ;
#1874 = DIRECTION ( 'NONE',  ( -6.938893903907228378E-16, 0.000000000000000000, 1.000000000000000000 ) ) ;
#1875 = VERTEX_POINT ( 'NONE', #3016 ) ;
#1876 = EDGE_CURVE ( 'NONE', #3215, #121, #1946, .T. ) ;
#1877 = ORIENTED_EDGE ( 'NONE', *, *, #1160, .T. ) ;
#1878 = DIRECTION ( 'NONE',  ( 0.000000000000000000, -0.000000000000000000, -1.000000000000000000 ) ) ;
#1879 = DIRECTION ( 'NONE',  ( 1.000000000000000000, 0.000000000000000000, -0.000000000000000000 ) ) ;
#1880 = EDGE_LOOP ( 'NONE', ( #763, #999 ) ) ;
#1881 = DIRECTION ( 'NONE',  ( -1.387778780781445676E-16, -0.000000000000000000, 1.000000000000000000 ) ) ;
#1882 = DIRECTION ( 'NONE',  ( 0.000000000000000000, 0.000000000000000000, 1.000000000000000000 ) ) ;
#1883 = EDGE_LOOP ( 'NONE', ( #1982, #2294, #933, #2811 ) ) ;
#1884 = DIRECTION ( 'NONE',  ( 1.000000000000000000, 0.000000000000000000, 0.000000000000000000 ) ) ;
#1885 = EDGE_CURVE ( 'NONE', #1696, #871, #1244, .T. ) ;
#1886 = DIRECTION ( 'NONE',  ( 0.000000000000000000, 0.000000000000000000, 1.000000000000000000 ) ) ;
#1887 = LINE ( 'NONE', #1666, #912 ) ;
#1888 = LINE ( 'NONE', #1415, #3220 ) ;
#1889 = ORIENTED_EDGE ( 'NONE', *, *, #3125, .T. ) ;
#1890 = ORIENTED_EDGE ( 'NONE', *, *, #1431, .T. ) ;
#1891 = DIRECTION ( 'NONE',  ( 6.938893903907232322E-16, -0.000000000000000000, 1.000000000000000000 ) ) ;
#1892 = AXIS2_PLACEMENT_3D ( 'NONE', #990, #2031, #2808 ) ;
#1893 = CYLINDRICAL_SURFACE ( 'NONE', #2934, 2.000000000000000888 ) ;
#1894 = AXIS2_PLACEMENT_3D ( 'NONE', #1163, #3245, #896 ) ;
#1895 = CIRCLE ( 'NONE', #2601, 3.500000000000000000 ) ;
#1896 = ORIENTED_EDGE ( 'NONE', *, *, #2101, .T. ) ;
#1897 = CARTESIAN_POINT ( 'NONE',  ( 0.000000000000000000, 25.00000000000000000, 52.00000000000000000 ) ) ;
#1898 = AXIS2_PLACEMENT_3D ( 'NONE', #2730, #1137, #1421 ) ;
#1899 = CONICAL_SURFACE ( 'NONE', #428, 1.610000000000000098, 0.7853981633974652654 ) ;
#1900 = DIRECTION ( 'NONE',  ( 1.000000000000000000, 0.000000000000000000, 0.000000000000000000 ) ) ;
#1901 = AXIS2_PLACEMENT_3D ( 'NONE', #119, #2689, #1668 ) ;
#1902 = AXIS2_PLACEMENT_3D ( 'NONE', #3238, #58, #1106 ) ;
#1903 = EDGE_LOOP ( 'NONE', ( #2092, #852, #613, #255 ) ) ;
#1904 = CARTESIAN_POINT ( 'NONE',  ( 0.000000000000000000, -0.8865213383406694847, 1.535500000000001419 ) ) ;
#1905 = STYLED_ITEM ( 'NONE', ( #620 ), #479 ) ;
#1906 =( LENGTH_UNIT ( ) NAMED_UNIT ( * ) SI_UNIT ( .MILLI., .METRE. ) );
#1907 = LINE ( 'NONE', #2950, #2385 ) ;
#1908 = EDGE_CURVE ( 'NONE', #595, #859, #1689, .T. ) ;
#1909 = DIRECTION ( 'NONE',  ( 0.000000000000000000, -1.000000000000000000, 0.000000000000000000 ) ) ;
#1910 = DIRECTION ( 'NONE',  ( -0.000000000000000000, -1.000000000000000000, -0.000000000000000000 ) ) ;
#1911 = ORIENTED_EDGE ( 'NONE', *, *, #2324, .T. ) ;
#1912 = ORIENTED_EDGE ( 'NONE', *, *, #144, .T. ) ;
#1913 = EDGE_CURVE ( 'NONE', #788, #887, #3265, .T. ) ;
#1914 = VECTOR ( 'NONE', #1139, 1000.000000000000000 ) ;
#1915 = CARTESIAN_POINT ( 'NONE',  ( 66.99999999999997158, 0.000000000000000000, -41.99999999999999289 ) ) ;
#1916 = CARTESIAN_POINT ( 'NONE',  ( -49.99999999999999289, 52.00000000000000711, -4.999999999999995559 ) ) ;
#1917 = EDGE_LOOP ( 'NONE', ( #1365, #2615 ) ) ;
#1918 = FACE_OUTER_BOUND ( 'NONE', #1794, .T. ) ;
#1919 = DIRECTION ( 'NONE',  ( 0.000000000000000000, 0.000000000000000000, 1.000000000000000000 ) ) ;
#1920 = ORIENTED_EDGE ( 'NONE', *, *, #259, .T. ) ;
#1921 = ADVANCED_FACE ( 'NONE', ( #673 ), #661, .T. ) ;
#1922 = PLANE ( 'NONE',  #532 ) ;
#1923 = DIRECTION ( 'NONE',  ( 0.000000000000000000, 0.000000000000000000, 1.000000000000000000 ) ) ;
#1924 = CARTESIAN_POINT ( 'NONE',  ( -54.99999999999995026, 130.0000000000000000, 5.000000000000004441 ) ) ;
#1925 = LINE ( 'NONE', #1654, #324 ) ;
#1926 = VERTEX_POINT ( 'NONE', #1753 ) ;
#1927 = ORIENTED_EDGE ( 'NONE', *, *, #1481, .F. ) ;
#1928 = CARTESIAN_POINT ( 'NONE',  ( 45.00000000000000000, 50.00000000000000000, 7.999999999999992895 ) ) ;
#1929 = ADVANCED_FACE ( 'NONE', ( #2261 ), #2737, .F. ) ;
#1930 = PLANE ( 'NONE',  #2497 ) ;
#1931 = ORIENTED_EDGE ( 'NONE', *, *, #2848, .T. ) ;
#1932 = CARTESIAN_POINT ( 'NONE',  ( 44.99999999999999289, 43.79827876194489278, -10.00000000000000533 ) ) ;
#1933 = CARTESIAN_POINT ( 'NONE',  ( 45.00000000000000000, 56.00000000000000711, 9.999999999999994671 ) ) ;
#1934 = EDGE_LOOP ( 'NONE', ( #1505, #2516, #1795, #1237 ) ) ;
#1935 = FACE_OUTER_BOUND ( 'NONE', #3201, .T. ) ;
#1936 = CYLINDRICAL_SURFACE ( 'NONE', #3318, 7.500000000000000000 ) ;
#1937 = DIRECTION ( 'NONE',  ( 0.000000000000000000, 0.000000000000000000, 1.000000000000000000 ) ) ;
#1938 = DIRECTION ( 'NONE',  ( 0.000000000000000000, 0.000000000000000000, 1.000000000000000000 ) ) ;
#1939 = LINE ( 'NONE', #170, #1669 ) ;
#1940 = LINE ( 'NONE', #664, #3326 ) ;
#1941 = PLANE ( 'NONE',  #2068 ) ;
#1942 = VECTOR ( 'NONE', #2794, 1000.000000000000000 ) ;
#1943 = ORIENTED_EDGE ( 'NONE', *, *, #43, .T. ) ;
#1944 = CARTESIAN_POINT ( 'NONE',  ( -44.99999999999999289, 52.00000000000000711, 7.850000000000005862 ) ) ;
#1945 = EDGE_CURVE ( 'NONE', #309, #2394, #3248, .T. ) ;
#1946 = CIRCLE ( 'NONE', #1349, 2.499999999999995115 ) ;
#1947 = CIRCLE ( 'NONE', #861, 2.000000000000001776 ) ;
#1948 = EDGE_LOOP ( 'NONE', ( #682, #2323, #1659, #927 ) ) ;
#1949 = COLOUR_RGB ( '',0.8941176470588234615, 0.8941176470588234615, 0.8941176470588234615 ) ;
#1950 = EDGE_CURVE ( 'NONE', #108, #3133, #967, .T. ) ;
#1951 = DIRECTION ( 'NONE',  ( -1.000000000000000000, -0.000000000000000000, -0.000000000000000000 ) ) ;
#1952 = VECTOR ( 'NONE', #2971, 1000.000000000000000 ) ;
#1953 = FACE_OUTER_BOUND ( 'NONE', #162, .T. ) ;
#1954 = MECHANICAL_DESIGN_GEOMETRIC_PRESENTATION_REPRESENTATION (  '', ( #3274 ), #2771 ) ;
#1955 = DIRECTION ( 'NONE',  ( 0.000000000000000000, 0.000000000000000000, 1.000000000000000000 ) ) ;
#1956 = AXIS2_PLACEMENT_3D ( 'NONE', #2472, #368, #2457 ) ;
#1957 = FILL_AREA_STYLE_COLOUR ( '', #2999 ) ;
#1958 = CIRCLE ( 'NONE', #2888, 1.535500000000000087 ) ;
#1959 = ORIENTED_EDGE ( 'NONE', *, *, #2868, .T. ) ;
#1960 = EDGE_CURVE ( 'NONE', #2478, #3154, #1525, .T. ) ;
#1961 = CARTESIAN_POINT ( 'NONE',  ( -51.00000000000000711, 52.00000000000000711, 6.000000000000004441 ) ) ;
#1962 = MECHANICAL_DESIGN_GEOMETRIC_PRESENTATION_REPRESENTATION (  '', ( #438 ), #3116 ) ;
#1963 = CARTESIAN_POINT ( 'NONE',  ( -66.99999999999997158, -8.000000000000000000, 41.99999999999999289 ) ) ;
#1964 = CIRCLE ( 'NONE', #757, 2.000000000000001776 ) ;
#1965 = VERTEX_POINT ( 'NONE', #117 ) ;
#1966 = CARTESIAN_POINT ( 'NONE',  ( 2.000000000000000000, -0.8865213383406694847, 1.535500000000001419 ) ) ;
#1967 = PRODUCT_CONTEXT ( 'NONE', #2725, 'mechanical' ) ;
#1968 = VERTEX_POINT ( 'NONE', #1166 ) ;
#1969 = CARTESIAN_POINT ( 'NONE',  ( -54.99999999999995026, 130.0000000000000000, 5.000000000000004441 ) ) ;
#1970 = EDGE_CURVE ( 'NONE', #113, #277, #2199, .T. ) ;
#1971 = SURFACE_SIDE_STYLE ('',( #129 ) ) ;
#1972 = DIRECTION ( 'NONE',  ( 1.000000000000000000, 0.000000000000000000, -0.000000000000000000 ) ) ;
#1973 = FACE_OUTER_BOUND ( 'NONE', #102, .T. ) ;
#1974 = CYLINDRICAL_SURFACE ( 'NONE', #1691, 2.499999999999995115 ) ;
#1975 = ORIENTED_EDGE ( 'NONE', *, *, #1111, .T. ) ;
#1976 = CARTESIAN_POINT ( 'NONE',  ( -44.99999999999999289, 50.00000000000000000, 10.00000000000000533 ) ) ;
#1977 = PRODUCT_DEFINITION_SHAPE ( 'NONE', 'NONE',  #3197 ) ;
#1978 = LINE ( 'NONE', #1861, #1464 ) ;
#1979 = VERTEX_POINT ( 'NONE', #2533 ) ;
#1980 = DIRECTION ( 'NONE',  ( 0.000000000000000000, 0.000000000000000000, 1.000000000000000000 ) ) ;
#1981 = APPLICATION_PROTOCOL_DEFINITION ( 'draft international standard', 'automotive_design', 1998, #112 ) ;
#1982 = ORIENTED_EDGE ( 'NONE', *, *, #2514, .T. ) ;
#1983 = DIRECTION ( 'NONE',  ( 0.000000000000000000, 0.000000000000000000, 1.000000000000000000 ) ) ;
#1984 = ORIENTED_EDGE ( 'NONE', *, *, #949, .T. ) ;
#1985 = DIRECTION ( 'NONE',  ( 0.000000000000000000, 0.000000000000000000, 1.000000000000000000 ) ) ;
#1986 = LINE ( 'NONE', #938, #3167 ) ;
#1987 = EDGE_CURVE ( 'NONE', #229, #1994, #766, .T. ) ;
#1988 = CARTESIAN_POINT ( 'NONE',  ( 66.99999999999997158, -5.000000000000000000, 39.50000000000000000 ) ) ;
#1989 = DIRECTION ( 'NONE',  ( 0.000000000000000000, 0.000000000000000000, 1.000000000000000000 ) ) ;
#1990 = PLANE ( 'NONE',  #976 ) ;
#1991 = EDGE_CURVE ( 'NONE', #824, #2761, #2790, .T. ) ;
#1992 = MANIFOLD_SOLID_BREP ( 'Boss-Extrude1', #2753 ) ;
#1993 = CARTESIAN_POINT ( 'NONE',  ( -66.99999999999997158, -6.000000000000000000, 41.99999999999999289 ) ) ;
#1994 = VERTEX_POINT ( 'NONE', #194 ) ;
#1995 = CARTESIAN_POINT ( 'NONE',  ( -45.00000000000000000, 45.00000000000000711, -9.999999999999994671 ) ) ;
#1996 = DIRECTION ( 'NONE',  ( -1.000000000000000000, 0.000000000000000000, 0.000000000000000000 ) ) ;
#1997 = ORIENTED_EDGE ( 'NONE', *, *, #1387, .F. ) ;
#1998 = EDGE_CURVE ( 'NONE', #480, #1538, #728, .T. ) ;
#1999 = CARTESIAN_POINT ( 'NONE',  ( 2.000000000000000000, 0.8865213383406680414, -1.535500000000000975 ) ) ;
#2000 = AXIS2_PLACEMENT_3D ( 'NONE', #3029, #1734, #3279 ) ;
#2001 = AXIS2_PLACEMENT_3D ( 'NONE', #1114, #1391, #1832 ) ;
#2002 = VECTOR ( 'NONE', #265, 1000.000000000000000 ) ;
#2003 = VERTEX_POINT ( 'NONE', #1314 ) ;
#2004 = PLANE ( 'NONE',  #3155 ) ;
#2005 = CARTESIAN_POINT ( 'NONE',  ( -45.00000000000000000, 52.00000000000000711, -7.849999999999996092 ) ) ;
#2006 = AXIS2_PLACEMENT_3D ( 'NONE', #2957, #1370, #612 ) ;
#2007 = AXIS2_PLACEMENT_3D ( 'NONE', #2593, #2343, #8 ) ;
#2008 = DIRECTION ( 'NONE',  ( 0.000000000000000000, 0.000000000000000000, -1.000000000000000000 ) ) ;
#2009=STYLED_ITEM('',(#3415),#2820);
#2010 = AXIS2_PLACEMENT_3D ( 'NONE', #712, #1413, #1955 ) ;
#2011 = DIRECTION ( 'NONE',  ( 0.000000000000000000, -1.000000000000000000, 0.000000000000000000 ) ) ;
#2012 = DIRECTION ( 'NONE',  ( 1.049727191138620668E-16, 0.5150380749100514910, -0.8571673007021138879 ) ) ;
#2013 = AXIS2_PLACEMENT_3D ( 'NONE', #521, #1060, #17 ) ;
#2014 = FACE_OUTER_BOUND ( 'NONE', #513, .T. ) ;
#2015 = EDGE_CURVE ( 'NONE', #1979, #2597, #1059, .T. ) ;
#2016 = ORIENTED_EDGE ( 'NONE', *, *, #1913, .T. ) ;
#2017 = ORIENTED_EDGE ( 'NONE', *, *, #3311, .T. ) ;
#2018 = PRESENTATION_LAYER_ASSIGNMENT (  '', '', ( #2235 ) ) ;
#2019 = DIRECTION ( 'NONE',  ( 0.000000000000000000, 0.000000000000000000, 1.000000000000000000 ) ) ;
#2020 = PRODUCT_DEFINITION_FORMATION_WITH_SPECIFIED_SOURCE ( 'ANY', '', #2551, .NOT_KNOWN. ) ;
#2021 = MANIFOLD_SOLID_BREP ( 'Boss-Extrude1', #2700 ) ;
#2022 = ITEM_DEFINED_TRANSFORMATION ( 'NONE', 'NONE', #497,  #3111 ) ;
#2023 = ORIENTED_EDGE ( 'NONE', *, *, #2417, .F. ) ;
#2024 = FACE_OUTER_BOUND ( 'NONE', #2788, .T. ) ;
#2025 = PRODUCT_DEFINITION ( 'UNKNOWN', '', #988, #240 ) ;
#2026 = VERTEX_POINT ( 'NONE', #3139 ) ;
#2027 = CYLINDRICAL_SURFACE ( 'NONE', #1732, 7.500000000000000000 ) ;
#2028 = CARTESIAN_POINT ( 'NONE',  ( 44.99999999999999289, 50.00000000000000000, -8.000000000000003553 ) ) ;
#2029 =( NAMED_UNIT ( * ) SI_UNIT ( $, .STERADIAN. ) SOLID_ANGLE_UNIT ( ) );
#2030 = APPLICATION_CONTEXT ( 'automotive_design' ) ;
#2031 = DIRECTION ( 'NONE',  ( -0.000000000000000000, 1.000000000000000000, -0.000000000000000000 ) ) ;
#2032 = DIRECTION ( 'NONE',  ( -0.000000000000000000, 1.000000000000000000, -0.000000000000000000 ) ) ;
#2033 = SURFACE_SIDE_STYLE ('',( #2742 ) ) ;
#2034 = ORIENTED_EDGE ( 'NONE', *, *, #691, .T. ) ;
#2035 = ORIENTED_EDGE ( 'NONE', *, *, #1779, .T. ) ;
#2036 = CARTESIAN_POINT ( 'NONE',  ( 0.000000000000000000, 4.163799117101000559E-16, -3.299999999999999822 ) ) ;
#2037 = EDGE_CURVE ( 'NONE', #740, #1843, #2171, .T. ) ;
#2038 = EDGE_LOOP ( 'NONE', ( #1777, #188, #2145, #628 ) ) ;
#2039 = PRODUCT_DEFINITION_SHAPE ( 'NONE', 'NONE',  #1526 ) ;
#2040 = ORIENTED_EDGE ( 'NONE', *, *, #2348, .F. ) ;
#2041 = DIRECTION ( 'NONE',  ( 0.000000000000000000, 0.000000000000000000, 1.000000000000000000 ) ) ;
#2042 =( NAMED_UNIT ( * ) PLANE_ANGLE_UNIT ( ) SI_UNIT ( $, .RADIAN. ) );
#2043 = ORIENTED_EDGE ( 'NONE', *, *, #1369, .T. ) ;
#2044 = CARTESIAN_POINT ( 'NONE',  ( -66.99999999999997158, 0.000000000000000000, -39.50000000000000000 ) ) ;
#2045 = CARTESIAN_POINT ( 'NONE',  ( 2.000000000000000000, 1.880445160090761061E-16, -1.535500000000000087 ) ) ;
#2046 = CARTESIAN_POINT ( 'NONE',  ( -50.00000000000000000, 120.0000000000000142, 5.000000000000004441 ) ) ;
#2047 = CARTESIAN_POINT ( 'NONE',  ( 2.000000000000000000, -1.329782007511007169, -0.7677499999999988223 ) ) ;
#2048 = DIRECTION ( 'NONE',  ( 1.000000000000000000, 0.000000000000000000, -6.938893903907232322E-16 ) ) ;
#2049 = EDGE_LOOP ( 'NONE', ( #2469, #124 ) ) ;
#2050 = ORIENTED_EDGE ( 'NONE', *, *, #1276, .T. ) ;
#2051 = FACE_BOUND ( 'NONE', #1917, .T. ) ;
#2052 = PRODUCT_DEFINITION_CONTEXT ( 'detailed design', #396, 'design' ) ;
#2053 = CONTEXT_DEPENDENT_SHAPE_REPRESENTATION ( #2767, #2123 ) ;
#2054 = VERTEX_POINT ( 'NONE', #1003 ) ;
#2055 = EDGE_CURVE ( 'NONE', #2072, #2365, #2081, .T. ) ;
#2056 = CARTESIAN_POINT ( 'NONE',  ( -66.99999999999997158, -5.000000000000000000, -41.99999999999999289 ) ) ;
#2057 = ORIENTED_EDGE ( 'NONE', *, *, #2082, .T. ) ;
#2058 = VECTOR ( 'NONE', #2627, 1000.000000000000000 ) ;
#2059 = FILL_AREA_STYLE ('',( #743 ) ) ;
#2060 = VECTOR ( 'NONE', #3192, 1000.000000000000114 ) ;
#2061 = CIRCLE ( 'NONE', #584, 2.000000000000001776 ) ;
#2062 = DIRECTION ( 'NONE',  ( 0.000000000000000000, 0.000000000000000000, -1.000000000000000000 ) ) ;
#2063 = CARTESIAN_POINT ( 'NONE',  ( -49.99999999999999289, 120.0000000000000142, -4.999999999999995559 ) ) ;
#2064 = VECTOR ( 'NONE', #1768, 1000.000000000000000 ) ;
#2065 = CARTESIAN_POINT ( 'NONE',  ( 66.99999999999997158, -5.000000000000000000, 41.99999999999999289 ) ) ;
#2066 = VECTOR ( 'NONE', #668, 1000.000000000000114 ) ;
#2067 = CARTESIAN_POINT ( 'NONE',  ( -66.99999999999997158, -6.000000000000000000, 41.99999999999999289 ) ) ;
#2068 = AXIS2_PLACEMENT_3D ( 'NONE', #2987, #73, #397 ) ;
#2069 = CIRCLE ( 'NONE', #591, 2.200000000000001066 ) ;
#2070 = ORIENTED_EDGE ( 'NONE', *, *, #2876, .T. ) ;
#2071 = ADVANCED_FACE ( 'NONE', ( #1783 ), #860, .T. ) ;
#2072 = VERTEX_POINT ( 'NONE', #1631 ) ;
#2073 = DIRECTION ( 'NONE',  ( -0.5000000000000061062, 0.000000000000000000, 0.8660254037844351549 ) ) ;
#2074 = AXIS2_PLACEMENT_3D ( 'NONE', #3285, #1773, #696 ) ;
#2075 = CONICAL_SURFACE ( 'NONE', #1853, 2.000000000000001776, 1.029744258676657642 ) ;
#2076 = ORIENTED_EDGE ( 'NONE', *, *, #2037, .T. ) ;
#2077 = DIRECTION ( 'NONE',  ( -0.000000000000000000, 1.000000000000000000, -0.000000000000000000 ) ) ;
#2078 = VERTEX_POINT ( 'NONE', #2684 ) ;
#2079 = DIRECTION ( 'NONE',  ( 0.000000000000000000, 0.000000000000000000, -1.000000000000000000 ) ) ;
#2080 = CARTESIAN_POINT ( 'NONE',  ( -66.99999999999997158, -6.000000000000000000, 41.99999999999999289 ) ) ;
#2081 = LINE ( 'NONE', #2045, #807 ) ;
#2082 = EDGE_CURVE ( 'NONE', #2103, #2003, #2988, .T. ) ;
#2083 = DIRECTION ( 'NONE',  ( 1.000000000000000000, 0.000000000000000000, -0.000000000000000000 ) ) ;
#2084 = DIRECTION ( 'NONE',  ( 0.000000000000000000, 0.000000000000000000, 1.000000000000000000 ) ) ;
#2085 = ORIENTED_EDGE ( 'NONE', *, *, #1369, .F. ) ;
#2086 = VERTEX_POINT ( 'NONE', #2160 ) ;
#2087 = CARTESIAN_POINT ( 'NONE',  ( 2.000000000000000000, -0.8865213383406730374, -1.535499999999999421 ) ) ;
#2088 = ADVANCED_FACE ( 'NONE', ( #813 ), #1327, .F. ) ;
#2089 = ORIENTED_EDGE ( 'NONE', *, *, #2696, .F. ) ;
#2090 = DIRECTION ( 'NONE',  ( -0.000000000000000000, 1.000000000000000000, -0.000000000000000000 ) ) ;
#2091 = UNCERTAINTY_MEASURE_WITH_UNIT (LENGTH_MEASURE( 1.000000000000000082E-05 ), #3069, 'distance_accuracy_value', 'NONE');
#2092 = ORIENTED_EDGE ( 'NONE', *, *, #783, .F. ) ;
#2093 = DIRECTION ( 'NONE',  ( 0.000000000000000000, -0.4999999999999991118, 0.8660254037844391517 ) ) ;
#2094 =( NAMED_UNIT ( * ) SI_UNIT ( $, .STERADIAN. ) SOLID_ANGLE_UNIT ( ) );
#2095 = FACE_OUTER_BOUND ( 'NONE', #982, .T. ) ;
#2096 = PLANE ( 'NONE',  #1507 ) ;
#2097 = EDGE_CURVE ( 'NONE', #2078, #2054, #45, .T. ) ;
#2098 = CARTESIAN_POINT ( 'NONE',  ( 45.00000000000000000, 45.00000000000000711, 9.999999999999994671 ) ) ;
#2099 = EDGE_LOOP ( 'NONE', ( #3068, #856, #1486, #476 ) ) ;
#2100 = VERTEX_POINT ( 'NONE', #604 ) ;
#2101 = EDGE_CURVE ( 'NONE', #684, #3122, #29, .T. ) ;
#2102 = FACE_BOUND ( 'NONE', #3090, .T. ) ;
#2103 = VERTEX_POINT ( 'NONE', #348 ) ;
#2104 = PLANE ( 'NONE',  #3043 ) ;
#2105 = CLOSED_SHELL ( 'NONE', ( #2661, #1815, #1341, #1616, #2638, #1043, #1052, #879, #960, #2738 ) ) ;
#2106 = VERTEX_POINT ( 'NONE', #2874 ) ;
#2107 = EDGE_CURVE ( 'NONE', #608, #2683, #316, .T. ) ;
#2108 = CARTESIAN_POINT ( 'NONE',  ( 0.000000000000000000, 25.00000000000000000, 47.00000000000000000 ) ) ;
#2109 = VECTOR ( 'NONE', #2847, 1000.000000000000000 ) ;
#2110 = LINE ( 'NONE', #1130, #2873 ) ;
#2111 = CARTESIAN_POINT ( 'NONE',  ( -75.00000000000000000, 50.00000000000000000, 50.00000000000000000 ) ) ;
#2112 = AXIS2_PLACEMENT_3D ( 'NONE', #406, #2979, #1460 ) ;
#2113 = AXIS2_PLACEMENT_3D ( 'NONE', #2964, #3002, #621 ) ;
#2114 = SURFACE_STYLE_FILL_AREA ( #1079 ) ;
#2115 = VERTEX_POINT ( 'NONE', #1359 ) ;
#2116 = AXIS2_PLACEMENT_3D ( 'NONE', #2998, #2483, #657 ) ;
#2117 = VECTOR ( 'NONE', #3309, 1000.000000000000000 ) ;
#2118 = ORIENTED_EDGE ( 'NONE', *, *, #1535, .F. ) ;
#2119 = DIRECTION ( 'NONE',  ( 0.000000000000000000, -1.000000000000000000, 0.000000000000000000 ) ) ;
#2120 = AXIS2_PLACEMENT_3D ( 'NONE', #2056, #2598, #504 ) ;
#2121 = VECTOR ( 'NONE', #784, 1000.000000000000000 ) ;
#2122 = ADVANCED_FACE ( 'NONE', ( #1612 ), #845, .F. ) ;
#2123 = PRODUCT_DEFINITION_SHAPE ( 'NONE', 'NONE',  #3382 ) ;
#2124 = ORIENTED_EDGE ( 'NONE', *, *, #1845, .T. ) ;
#2125 = CIRCLE ( 'NONE', #2074, 2.000000000000001776 ) ;
#2126 = VECTOR ( 'NONE', #3194, 1000.000000000000000 ) ;
#2127 = CARTESIAN_POINT ( 'NONE',  ( -66.99999999999997158, -5.000000000000000000, 44.49999999999999289 ) ) ;
#2128 =( GEOMETRIC_REPRESENTATION_CONTEXT ( 3 ) GLOBAL_UNCERTAINTY_ASSIGNED_CONTEXT ( ( #553 ) ) GLOBAL_UNIT_ASSIGNED_CONTEXT ( ( #1906, #1613, #2414 ) ) REPRESENTATION_CONTEXT ( 'NONE', 'WORKASPACE' ) );
#2129 = VERTEX_POINT ( 'NONE', #1649 ) ;
#2130 = MECHANICAL_DESIGN_GEOMETRIC_PRESENTATION_REPRESENTATION (  '', ( #985 ), #1263 ) ;
#2131 = DIRECTION ( 'NONE',  ( 1.000000000000000000, 0.000000000000000000, 0.000000000000000000 ) ) ;
#2132 = EDGE_CURVE ( 'NONE', #3190, #531, #917, .T. ) ;
#2133 =( NAMED_UNIT ( * ) PLANE_ANGLE_UNIT ( ) SI_UNIT ( $, .RADIAN. ) );
#2134 = VECTOR ( 'NONE', #1477, 1000.000000000000000 ) ;
#2135 = DIRECTION ( 'NONE',  ( 0.000000000000000000, 0.000000000000000000, -1.000000000000000000 ) ) ;
#2136 = DIRECTION ( 'NONE',  ( 0.000000000000000000, 0.5150380749100514910, 0.8571673007021138879 ) ) ;
#2137 = CARTESIAN_POINT ( 'NONE',  ( 6.812556682370379590, 25.00000000000000000, 52.00000000000000000 ) ) ;
#2138 = ORIENTED_EDGE ( 'NONE', *, *, #1021, .F. ) ;
#2139 = EDGE_LOOP ( 'NONE', ( #582, #2167, #2852, #1087 ) ) ;
#2140 = DIRECTION ( 'NONE',  ( 0.000000000000000000, 0.000000000000000000, -1.000000000000000000 ) ) ;
#2141 = FACE_OUTER_BOUND ( 'NONE', #2666, .T. ) ;
#2142 = ORIENTED_EDGE ( 'NONE', *, *, #2720, .T. ) ;
#2143 = EDGE_CURVE ( 'NONE', #489, #1297, #317, .T. ) ;
#2144 = DIRECTION ( 'NONE',  ( 0.000000000000000000, 0.000000000000000000, 1.000000000000000000 ) ) ;
#2145 = ORIENTED_EDGE ( 'NONE', *, *, #2143, .T. ) ;
#2146 = CARTESIAN_POINT ( 'NONE',  ( -40.00000000000000000, 52.00000000000000711, 5.000000000000000888 ) ) ;
#2147 = FILL_AREA_STYLE_COLOUR ( '', #1470 ) ;
#2148 = DIRECTION ( 'NONE',  ( 0.000000000000000000, 0.000000000000000000, -1.000000000000000000 ) ) ;
#2149 = LINE ( 'NONE', #2383, #201 ) ;
#2150 = FACE_OUTER_BOUND ( 'NONE', #2581, .T. ) ;
#2151 = ORIENTED_EDGE ( 'NONE', *, *, #2906, .F. ) ;
#2152 = ORIENTED_EDGE ( 'NONE', *, *, #777, .F. ) ;
#2153 = DIRECTION ( 'NONE',  ( -1.000000000000000000, 0.000000000000000000, -0.000000000000000000 ) ) ;
#2154 = DIRECTION ( 'NONE',  ( -1.000000000000000000, -0.000000000000000000, -0.000000000000000000 ) ) ;
#2155 = ORIENTED_EDGE ( 'NONE', *, *, #646, .F. ) ;
#2156 = CARTESIAN_POINT ( 'NONE',  ( -31.74999999999995737, 0.000000000000000000, 0.000000000000000000 ) ) ;
#2157 = ADVANCED_FACE ( 'NONE', ( #2895 ), #2822, .F. ) ;
#2158 = CARTESIAN_POINT ( 'NONE',  ( 0.000000000000000000, 0.000000000000000000, 0.000000000000000000 ) ) ;
#2159 = ORIENTED_EDGE ( 'NONE', *, *, #535, .F. ) ;
#2160 = CARTESIAN_POINT ( 'NONE',  ( -44.99999999999999289, 43.79827876194489278, 10.00000000000000533 ) ) ;
#2161 = ADVANCED_FACE ( 'NONE', ( #2400 ), #1731, .F. ) ;
#2162 = CARTESIAN_POINT ( 'NONE',  ( 10.00000000000000178, 0.000000000000000000, 1.610000000000000098 ) ) ;
#2163 =( REPRESENTATION_RELATIONSHIP ('NONE','NONE', #3165, #1286 ) REPRESENTATION_RELATIONSHIP_WITH_TRANSFORMATION ( #3093 )SHAPE_REPRESENTATION_RELATIONSHIP( ) );
#2164 = PLANE ( 'NONE',  #1414 ) ;
#2165 = DIRECTION ( 'NONE',  ( -0.000000000000000000, 1.000000000000000000, -0.000000000000000000 ) ) ;
#2166 = ORIENTED_EDGE ( 'NONE', *, *, #2576, .T. ) ;
#2167 = ORIENTED_EDGE ( 'NONE', *, *, #997, .T. ) ;
#2168 = DIRECTION ( 'NONE',  ( 0.000000000000000000, 0.000000000000000000, -1.000000000000000000 ) ) ;
#2169 = AXIS2_PLACEMENT_3D ( 'NONE', #1077, #319, #2148 ) ;
#2170 = CARTESIAN_POINT ( 'NONE',  ( 44.99999999999999289, 45.00000000000000711, -10.00000000000000533 ) ) ;
#2171 = CIRCLE ( 'NONE', #2658, 2.149999999999999023 ) ;
#2172 = EDGE_CURVE ( 'NONE', #575, #2435, #79, .T. ) ;
#2173 = VECTOR ( 'NONE', #893, 1000.000000000000000 ) ;
#2174 = VERTEX_POINT ( 'NONE', #2182 ) ;
#2175 = CARTESIAN_POINT ( 'NONE',  ( -40.00000000000000000, 52.00000000000000711, 5.000000000000004441 ) ) ;
#2176 = AXIS2_PLACEMENT_3D ( 'NONE', #2170, #3222, #875 ) ;
#2177 = AXIS2_PLACEMENT_3D ( 'NONE', #3138, #110, #2465 ) ;
#2178 = DIRECTION ( 'NONE',  ( 1.000000000000000000, 0.000000000000000000, 0.000000000000000000 ) ) ;
#2179 = CIRCLE ( 'NONE', #648, 2.000000000000000888 ) ;
#2180 = AXIS2_PLACEMENT_3D ( 'NONE', #198, #1722, #2757 ) ;
#2181 = ORIENTED_EDGE ( 'NONE', *, *, #416, .T. ) ;
#2182 = CARTESIAN_POINT ( 'NONE',  ( -40.00000000000000000, 52.00000000000000711, -4.999999999999996447 ) ) ;
#2183 = VECTOR ( 'NONE', #3297, 1000.000000000000000 ) ;
#2184 = DIRECTION ( 'NONE',  ( -1.000000000000000000, 0.000000000000000000, 4.857225732735056709E-15 ) ) ;
#2185 = DIRECTION ( 'NONE',  ( -0.000000000000000000, -1.000000000000000000, -0.000000000000000000 ) ) ;
#2186 = EDGE_CURVE ( 'NONE', #1751, #624, #2547, .T. ) ;
#2187 = CARTESIAN_POINT ( 'NONE',  ( -66.99999999999997158, -5.000000000000000000, -39.50000000000000000 ) ) ;
#2188 = EDGE_LOOP ( 'NONE', ( #2310, #1604 ) ) ;
#2189 = ORIENTED_EDGE ( 'NONE', *, *, #3017, .T. ) ;
#2190 = CARTESIAN_POINT ( 'NONE',  ( 2.000000000000000000, 2.065682573263594481E-15, 1.535500000000000309 ) ) ;
#2191 = FACE_OUTER_BOUND ( 'NONE', #1498, .T. ) ;
#2192 = EDGE_LOOP ( 'NONE', ( #2885, #1417 ) ) ;
#2193 = LINE ( 'NONE', #1372, #1142 ) ;
#2194 = PRODUCT_RELATED_PRODUCT_CATEGORY ( 'part', '', ( #25 ) ) ;
#2195 = SHAPE_DEFINITION_REPRESENTATION ( #3103, #714 ) ;
#2196 = ORIENTED_EDGE ( 'NONE', *, *, #1607, .T. ) ;
#2197 = LINE ( 'NONE', #2977, #2134 ) ;
#2198 = CARTESIAN_POINT ( 'NONE',  ( -66.99999999999997158, -5.000000000000000000, -44.49999999999999289 ) ) ;
#2199 = LINE ( 'NONE', #2028, #3095 ) ;
#2200 = DIRECTION ( 'NONE',  ( -0.000000000000000000, -1.000000000000000000, -0.000000000000000000 ) ) ;
#2201 = ADVANCED_FACE ( 'NONE', ( #3204 ), #3039, .F. ) ;
#2202 = EDGE_LOOP ( 'NONE', ( #812, #2681, #3113, #1321 ) ) ;
#2203 = FACE_OUTER_BOUND ( 'NONE', #1591, .T. ) ;
#2204 = DIRECTION ( 'NONE',  ( 0.000000000000000000, 0.000000000000000000, 1.000000000000000000 ) ) ;
#2205 = EDGE_CURVE ( 'NONE', #2259, #277, #1571, .T. ) ;
#2206 = ORIENTED_EDGE ( 'NONE', *, *, #2257, .T. ) ;
#2207 = DIRECTION ( 'NONE',  ( 0.000000000000000000, -1.000000000000000000, 0.000000000000000000 ) ) ;
#2208 = APPLICATION_PROTOCOL_DEFINITION ( 'draft international standard', 'automotive_design', 1998, #287 ) ;
#2209 = ORIENTED_EDGE ( 'NONE', *, *, #325, .F. ) ;
#2210 = CARTESIAN_POINT ( 'NONE',  ( -50.00000000000000000, 52.00000000000000711, 5.000000000000004441 ) ) ;
#2211 = EDGE_CURVE ( 'NONE', #2585, #35, #2625, .T. ) ;
#2212 = CARTESIAN_POINT ( 'NONE',  ( 75.00000000000000000, 50.00000000000000000, -50.00000000000000000 ) ) ;
#2213 = CARTESIAN_POINT ( 'NONE',  ( -44.99999999999999289, 52.00000000000000711, 12.15000000000000391 ) ) ;
#2214 = DIRECTION ( 'NONE',  ( 1.000000000000000000, 0.000000000000000000, 0.000000000000000000 ) ) ;
#2215 = CARTESIAN_POINT ( 'NONE',  ( -40.00000000000000000, 136.9705627484771355, 5.000000000000004441 ) ) ;
#2216 = DIRECTION ( 'NONE',  ( 0.000000000000000000, 0.000000000000000000, -1.000000000000000000 ) ) ;
#2217 = ORIENTED_EDGE ( 'NONE', *, *, #1742, .T. ) ;
#2218 = LINE ( 'NONE', #2541, #2877 ) ;
#2219 = EDGE_CURVE ( 'NONE', #1968, #2106, #3322, .T. ) ;
#2220=STYLED_ITEM('',(#3408),#1992);
#2221 = DIRECTION ( 'NONE',  ( -1.000000000000000000, 0.000000000000000000, 0.000000000000000000 ) ) ;
#2222 = VERTEX_POINT ( 'NONE', #1700 ) ;
#2223 = AXIS2_PLACEMENT_3D ( 'NONE', #1664, #2515, #2699 ) ;
#2224 = VECTOR ( 'NONE', #193, 1000.000000000000000 ) ;
#2225 = PLANE ( 'NONE',  #2223 ) ;
#2226 = CIRCLE ( 'NONE', #1519, 2.000000000000001776 ) ;
#2227 = AXIS2_PLACEMENT_3D ( 'NONE', #798, #252, #3372 ) ;
#2228 = PLANE ( 'NONE',  #2000 ) ;
#2229 = VECTOR ( 'NONE', #1318, 1000.000000000000000 ) ;
#2230 = DIRECTION ( 'NONE',  ( 0.000000000000000000, 0.000000000000000000, 1.000000000000000000 ) ) ;
#2231 =( LENGTH_UNIT ( ) NAMED_UNIT ( * ) SI_UNIT ( .MILLI., .METRE. ) );
#2232 = AXIS2_PLACEMENT_3D ( 'NONE', #217, #2332, #2555 ) ;
#2233 = CARTESIAN_POINT ( 'NONE',  ( -51.00000000000000711, 117.0000000000000000, 6.000000000000004441 ) ) ;
#2234 = CARTESIAN_POINT ( 'NONE',  ( -39.00000000000000000, 52.00000000000000711, 6.000000000000004441 ) ) ;
#2235 = STYLED_ITEM ( 'NONE', ( #1730 ), #315 ) ;
#2236 = CARTESIAN_POINT ( 'NONE',  ( -44.99999999999999289, 45.00000000000000711, 8.000000000000003553 ) ) ;
#2237 = EDGE_LOOP ( 'NONE', ( #74, #245, #2450, #2549 ) ) ;
#2238 = PLANE ( 'NONE',  #641 ) ;
#2239 = VERTEX_POINT ( 'NONE', #1225 ) ;
#2240 = EDGE_CURVE ( 'NONE', #1531, #1041, #881, .T. ) ;
#2241 = DIRECTION ( 'NONE',  ( -1.000000000000000000, 0.000000000000000000, -0.000000000000000000 ) ) ;
#2242 = ORIENTED_EDGE ( 'NONE', *, *, #409, .F. ) ;
#2243 = EDGE_CURVE ( 'NONE', #2597, #880, #363, .T. ) ;
#2244 = LINE ( 'NONE', #1665, #2494 ) ;
#2245 = LINE ( 'NONE', #3030, #540 ) ;
#2246 =( REPRESENTATION_RELATIONSHIP ('NONE','NONE', #3165, #2804 ) REPRESENTATION_RELATIONSHIP_WITH_TRANSFORMATION ( #207 )SHAPE_REPRESENTATION_RELATIONSHIP( ) );
#2247 = CARTESIAN_POINT ( 'NONE',  ( -49.99999999999999289, 117.0000000000000000, -4.999999999999995559 ) ) ;
#2248 = CARTESIAN_POINT ( 'NONE',  ( 75.00000000000000000, 0.000000000000000000, 50.00000000000000000 ) ) ;
#2249 = DIRECTION ( 'NONE',  ( 0.000000000000000000, 0.000000000000000000, -1.000000000000000000 ) ) ;
#2250 = PRODUCT_DEFINITION_SHAPE ( 'NONE', 'NONE',  #3381 ) ;
#2251 = SURFACE_STYLE_FILL_AREA ( #1758 ) ;
#2252 = VERTEX_POINT ( 'NONE', #1212 ) ;
#2253 = DIRECTION ( 'NONE',  ( -0.000000000000000000, 1.000000000000000000, -0.000000000000000000 ) ) ;
#2254 = DIRECTION ( 'NONE',  ( 6.123233995736766036E-17, -1.000000000000000000, 0.000000000000000000 ) ) ;
#2255 = ORIENTED_EDGE ( 'NONE', *, *, #1149, .F. ) ;
#2256 = DIRECTION ( 'NONE',  ( 1.000000000000000000, 0.000000000000000000, 0.000000000000000000 ) ) ;
#2257 = EDGE_CURVE ( 'NONE', #2106, #1319, #1453, .T. ) ;
#2258 = SURFACE_STYLE_FILL_AREA ( #1440 ) ;
#2259 = VERTEX_POINT ( 'NONE', #178 ) ;
#2260 = LINE ( 'NONE', #1002, #2117 ) ;
#2261 = FACE_OUTER_BOUND ( 'NONE', #1618, .T. ) ;
#2262 = EDGE_CURVE ( 'NONE', #531, #3190, #2930, .T. ) ;
#2263 = DIRECTION ( 'NONE',  ( 0.000000000000000000, -0.5000000000000011102, -0.8660254037844379305 ) ) ;
#2264 = CARTESIAN_POINT ( 'NONE',  ( 45.00000000000000000, 50.00000000000000000, 9.999999999999994671 ) ) ;
#2265 = LINE ( 'NONE', #1484, #2281 ) ;
#2266 = CIRCLE ( 'NONE', #1236, 3.299999999999999822 ) ;
#2267 = DIRECTION ( 'NONE',  ( -1.000000000000000000, -0.000000000000000000, -0.000000000000000000 ) ) ;
#2268 = ORIENTED_EDGE ( 'NONE', *, *, #891, .F. ) ;
#2269 = CYLINDRICAL_SURFACE ( 'NONE', #206, 2.499999999999995115 ) ;
#2270 = PRODUCT_DEFINITION ( 'UNKNOWN', '', #1748, #1030 ) ;
#2271 = AXIS2_PLACEMENT_3D ( 'NONE', #3085, #745, #730 ) ;
#2272 = ITEM_DEFINED_TRANSFORMATION ( 'NONE', 'NONE', #1105,  #3111 ) ;
#2273 = VERTEX_POINT ( 'NONE', #143 ) ;
#2274 = FACE_OUTER_BOUND ( 'NONE', #892, .T. ) ;
#2275 = PRESENTATION_LAYER_ASSIGNMENT (  '', '', ( #2440 ) ) ;
#2276 = VECTOR ( 'NONE', #2719, 1000.000000000000000 ) ;
#2277 = VECTOR ( 'NONE', #1881, 1000.000000000000000 ) ;
#2278 = ORIENTED_EDGE ( 'NONE', *, *, #1250, .F. ) ;
#2279 = DIRECTION ( 'NONE',  ( 0.000000000000000000, 0.000000000000000000, 1.000000000000000000 ) ) ;
#2280 = CIRCLE ( 'NONE', #427, 2.000000000000001776 ) ;
#2281 = VECTOR ( 'NONE', #2506, 1000.000000000000000 ) ;
#2282 = LINE ( 'NONE', #1216, #2183 ) ;
#2283 = PRESENTATION_LAYER_ASSIGNMENT (  '', '', ( #3274 ) ) ;
#2284 = VECTOR ( 'NONE', #2048, 1000.000000000000000 ) ;
#2285 = FACE_OUTER_BOUND ( 'NONE', #243, .T. ) ;
#2286 = ADVANCED_FACE ( 'NONE', ( #1935 ), #1922, .T. ) ;
#2287 = DIRECTION ( 'NONE',  ( 0.000000000000000000, 0.000000000000000000, -1.000000000000000000 ) ) ;
#2288 = VECTOR ( 'NONE', #729, 1000.000000000000000 ) ;
#2289 = FILL_AREA_STYLE_COLOUR ( '', #54 ) ;
#2290 = ORIENTED_EDGE ( 'NONE', *, *, #3213, .F. ) ;
#2291 = VERTEX_POINT ( 'NONE', #1439 ) ;
#2292 = CARTESIAN_POINT ( 'NONE',  ( 0.000000000000000000, 0.8865213383406680414, -1.535500000000000975 ) ) ;
#2293 = UNCERTAINTY_MEASURE_WITH_UNIT (LENGTH_MEASURE( 1.000000000000000082E-05 ), #911, 'distance_accuracy_value', 'NONE');
#2294 = ORIENTED_EDGE ( 'NONE', *, *, #1998, .F. ) ;
#2295 = DIRECTION ( 'NONE',  ( 0.000000000000000000, 0.000000000000000000, 1.000000000000000000 ) ) ;
#2296 =( NAMED_UNIT ( * ) PLANE_ANGLE_UNIT ( ) SI_UNIT ( $, .RADIAN. ) );
#2297 = ORIENTED_EDGE ( 'NONE', *, *, #2353, .T. ) ;
#2298 = DIRECTION ( 'NONE',  ( -1.000000000000000000, -0.000000000000000000, -0.000000000000000000 ) ) ;
#2299 = DIRECTION ( 'NONE',  ( -0.000000000000000000, 1.000000000000000000, -0.000000000000000000 ) ) ;
#2300 = LINE ( 'NONE', #30, #1098 ) ;
#2301 = DIRECTION ( 'NONE',  ( 0.000000000000000000, -1.000000000000000000, 0.000000000000000000 ) ) ;
#2302 = DIRECTION ( 'NONE',  ( 0.000000000000000000, -1.000000000000000000, 0.000000000000000000 ) ) ;
#2303 = EDGE_CURVE ( 'NONE', #1203, #2435, #2197, .T. ) ;
#2304 = DIRECTION ( 'NONE',  ( 1.000000000000000000, 0.000000000000000000, 0.000000000000000000 ) ) ;
#2305 = ORIENTED_EDGE ( 'NONE', *, *, #1960, .T. ) ;
#2306 = VERTEX_POINT ( 'NONE', #417 ) ;
#2307 = CARTESIAN_POINT ( 'NONE',  ( 4.200000000000001954, 0.000000000000000000, 0.000000000000000000 ) ) ;
#2308 = ADVANCED_FACE ( 'NONE', ( #2470 ), #2225, .F. ) ;
#2309 = CONTEXT_DEPENDENT_SHAPE_REPRESENTATION ( #1706, #838 ) ;
#2310 = ORIENTED_EDGE ( 'NONE', *, *, #1822, .F. ) ;
#2311 = FACE_OUTER_BOUND ( 'NONE', #2766, .T. ) ;
#2312 = ORIENTED_EDGE ( 'NONE', *, *, #2107, .F. ) ;
#2313 = CARTESIAN_POINT ( 'NONE',  ( 2.000000000000000000, 1.773042676681340524, -2.059984127722458425E-15 ) ) ;
#2314 = EDGE_CURVE ( 'NONE', #2435, #3240, #1428, .T. ) ;
#2315 = CARTESIAN_POINT ( 'NONE',  ( -66.99999999999997158, -5.000000000000000000, -39.50000000000000000 ) ) ;
#2316 = DIRECTION ( 'NONE',  ( 0.000000000000000000, 0.000000000000000000, -1.000000000000000000 ) ) ;
#2317 = DIRECTION ( 'NONE',  ( 0.000000000000000000, 0.000000000000000000, 1.000000000000000000 ) ) ;
#2318 = DIRECTION ( 'NONE',  ( 0.000000000000000000, 0.000000000000000000, -1.000000000000000000 ) ) ;
#2319 = ORIENTED_EDGE ( 'NONE', *, *, #205, .T. ) ;
#2320 = VERTEX_POINT ( 'NONE', #1408 ) ;
#2321 = FACE_OUTER_BOUND ( 'NONE', #987, .T. ) ;
#2322 = AXIS2_PLACEMENT_3D ( 'NONE', #923, #2780, #2705 ) ;
#2323 = ORIENTED_EDGE ( 'NONE', *, *, #789, .F. ) ;
#2324 = EDGE_CURVE ( 'NONE', #1554, #1763, #2451, .T. ) ;
#2325 = DIRECTION ( 'NONE',  ( -0.000000000000000000, -1.000000000000000000, -0.000000000000000000 ) ) ;
#2326 = SURFACE_STYLE_USAGE ( .BOTH. , #505 ) ;
#2327 = EDGE_LOOP ( 'NONE', ( #2734, #1801 ) ) ;
#2328 = AXIS2_PLACEMENT_3D ( 'NONE', #1146, #2927, #2135 ) ;
#2329 = CARTESIAN_POINT ( 'NONE',  ( -40.00000000000000000, 52.00000000000000711, 5.000000000000004441 ) ) ;
#2330 = AXIS2_PLACEMENT_3D ( 'NONE', #909, #2749, #388 ) ;
#2331 = AXIS2_PLACEMENT_3D ( 'NONE', #2431, #81, #2402 ) ;
#2332 = DIRECTION ( 'NONE',  ( 0.000000000000000000, -1.000000000000000000, 0.000000000000000000 ) ) ;
#2333 = DIRECTION ( 'NONE',  ( 1.000000000000000000, 0.000000000000000000, -2.365532012695647018E-17 ) ) ;
#2334 = EDGE_CURVE ( 'NONE', #190, #787, #1681, .T. ) ;
#2335 = DIRECTION ( 'NONE',  ( 0.000000000000000000, 0.000000000000000000, 1.000000000000000000 ) ) ;
#2336 = VECTOR ( 'NONE', #1825, 1000.000000000000000 ) ;
#2337 = PRODUCT_DEFINITION_SHAPE ( 'NONE', 'NONE',  #3374 ) ;
#2338 = FACE_OUTER_BOUND ( 'NONE', #3118, .T. ) ;
#2339 = VECTOR ( 'NONE', #2656, 1000.000000000000000 ) ;
#2340 = CIRCLE ( 'NONE', #322, 6.000000000000005329 ) ;
#2341 = EDGE_LOOP ( 'NONE', ( #2524, #1153, #2035 ) ) ;
#2342 = VERTEX_POINT ( 'NONE', #3291 ) ;
#2343 = DIRECTION ( 'NONE',  ( 1.000000000000000000, 0.000000000000000000, 0.000000000000000000 ) ) ;
#2344 = VECTOR ( 'NONE', #2263, 1000.000000000000114 ) ;
#2345 = VERTEX_POINT ( 'NONE', #2210 ) ;
#2346 = DIRECTION ( 'NONE',  ( -0.000000000000000000, 1.000000000000000000, -0.000000000000000000 ) ) ;
#2347 = AXIS2_PLACEMENT_3D ( 'NONE', #2158, #3227, #1900 ) ;
#2348 = EDGE_CURVE ( 'NONE', #3133, #2345, #634, .T. ) ;
#2349 = ORIENTED_EDGE ( 'NONE', *, *, #767, .F. ) ;
#2350 = EDGE_CURVE ( 'NONE', #2691, #594, #382, .T. ) ;
#2351 = DIRECTION ( 'NONE',  ( 0.000000000000000000, 0.000000000000000000, -1.000000000000000000 ) ) ;
#2352 = SURFACE_SIDE_STYLE ('',( #1532 ) ) ;
#2353 = EDGE_CURVE ( 'NONE', #1840, #3340, #422, .T. ) ;
#2354 = DIRECTION ( 'NONE',  ( 0.000000000000000000, -1.000000000000000000, 0.000000000000000000 ) ) ;
#2355 = CARTESIAN_POINT ( 'NONE',  ( -7.500000000000000000, 25.00000000000000000, 47.00000000000000000 ) ) ;
#2356 = CARTESIAN_POINT ( 'NONE',  ( -49.99999999999999289, 52.00000000000000711, 5.000000000000007994 ) ) ;
#2357 = DIRECTION ( 'NONE',  ( 0.000000000000000000, -1.000000000000000000, 0.000000000000000000 ) ) ;
#2358 = ORIENTED_EDGE ( 'NONE', *, *, #3058, .F. ) ;
#2359 = ORIENTED_EDGE ( 'NONE', *, *, #825, .T. ) ;
#2360 = CARTESIAN_POINT ( 'NONE',  ( 44.99999999999999289, 50.00000000000000000, -10.00000000000000533 ) ) ;
#2361 = ADVANCED_FACE ( 'NONE', ( #1188 ), #1177, .T. ) ;
#2362 = ORIENTED_EDGE ( 'NONE', *, *, #433, .F. ) ;
#2363 = LINE ( 'NONE', #27, #157 ) ;
#2364 = DIRECTION ( 'NONE',  ( 1.000000000000000000, 0.000000000000000000, 0.000000000000000000 ) ) ;
#2365 = VERTEX_POINT ( 'NONE', #683 ) ;
#2366 = PRODUCT_DEFINITION_SHAPE ( 'NONE', 'NONE',  #3373 ) ;
#2367 = DIRECTION ( 'NONE',  ( -0.000000000000000000, -1.000000000000000000, -0.000000000000000000 ) ) ;
#2368 = DIRECTION ( 'NONE',  ( -0.000000000000000000, 1.000000000000000000, -0.000000000000000000 ) ) ;
#2369 = PLANE ( 'NONE',  #2331 ) ;
#2370 = DIRECTION ( 'NONE',  ( 0.000000000000000000, -1.000000000000000000, 0.000000000000000000 ) ) ;
#2371 = ADVANCED_FACE ( 'NONE', ( #3277 ), #935, .F. ) ;
#2372 = FILL_AREA_STYLE_COLOUR ( '', #1849 ) ;
#2373 = ORIENTED_EDGE ( 'NONE', *, *, #90, .T. ) ;
#2374 = ORIENTED_EDGE ( 'NONE', *, *, #949, .F. ) ;
#2375 = PLANE ( 'NONE',  #1682 ) ;
#2376 = ORIENTED_EDGE ( 'NONE', *, *, #1276, .F. ) ;
#2377 = APPLICATION_CONTEXT ( 'automotive_design' ) ;
#2378 = EDGE_CURVE ( 'NONE', #820, #2026, #640, .T. ) ;
#2379 = LINE ( 'NONE', #2870, #1792 ) ;
#2380 = ORIENTED_EDGE ( 'NONE', *, *, #842, .F. ) ;
#2381 = DIRECTION ( 'NONE',  ( 0.000000000000000000, -0.000000000000000000, -1.000000000000000000 ) ) ;
#2382 = DIRECTION ( 'NONE',  ( 0.000000000000000000, 0.000000000000000000, 1.000000000000000000 ) ) ;
#2383 = CARTESIAN_POINT ( 'NONE',  ( -66.99999999999997158, -8.000000000000000000, 37.49999999999998579 ) ) ;
#2384 = AXIS2_PLACEMENT_3D ( 'NONE', #746, #2589, #1602 ) ;
#2385 = VECTOR ( 'NONE', #350, 1000.000000000000000 ) ;
#2386 = CYLINDRICAL_SURFACE ( 'NONE', #3172, 2.149999999999999023 ) ;
#2387 = ADVANCED_FACE ( 'NONE', ( #2545, #984, #1778, #1559, #2024 ), #466, .F. ) ;
#2388 = ORIENTED_EDGE ( 'NONE', *, *, #1908, .T. ) ;
#2389 = VECTOR ( 'NONE', #1710, 1000.000000000000000 ) ;
#2390 = ORIENTED_EDGE ( 'NONE', *, *, #1118, .T. ) ;
#2391 = DIRECTION ( 'NONE',  ( 0.000000000000000000, -1.000000000000000000, 0.000000000000000000 ) ) ;
#2392 = VECTOR ( 'NONE', #39, 1000.000000000000000 ) ;
#2393 = AXIS2_PLACEMENT_3D ( 'NONE', #889, #1672, #873 ) ;
#2394 = VERTEX_POINT ( 'NONE', #3119 ) ;
#2395 = VECTOR ( 'NONE', #560, 1000.000000000000000 ) ;
#2396 = DIRECTION ( 'NONE',  ( 0.000000000000000000, 0.000000000000000000, 1.000000000000000000 ) ) ;
#2397 = DIRECTION ( 'NONE',  ( 1.000000000000000000, 0.000000000000000000, 0.000000000000000000 ) ) ;
#2398 = VERTEX_POINT ( 'NONE', #1750 ) ;
#2399 =( GEOMETRIC_REPRESENTATION_CONTEXT ( 3 ) GLOBAL_UNCERTAINTY_ASSIGNED_CONTEXT ( ( #140 ) ) GLOBAL_UNIT_ASSIGNED_CONTEXT ( ( #3331, #2042, #3136 ) ) REPRESENTATION_CONTEXT ( 'NONE', 'WORKASPACE' ) );
#2400 = FACE_OUTER_BOUND ( 'NONE', #1774, .T. ) ;
#2401 = PRODUCT_DEFINITION_FORMATION_WITH_SPECIFIED_SOURCE ( 'ANY', '', #2796, .NOT_KNOWN. ) ;
#2402 = DIRECTION ( 'NONE',  ( -1.000000000000000000, 0.000000000000000000, -0.000000000000000000 ) ) ;
#2403 = CARTESIAN_POINT ( 'NONE',  ( 2.000000000000000000, 1.773042676681340524, -2.059984127722458425E-15 ) ) ;
#2404 = FACE_OUTER_BOUND ( 'NONE', #1645, .T. ) ;
#2405 = VERTEX_POINT ( 'NONE', #1262 ) ;
#2406 = ORIENTED_EDGE ( 'NONE', *, *, #603, .F. ) ;
#2407 = CARTESIAN_POINT ( 'NONE',  ( -49.99999999999999289, 52.00000000000000711, -14.99999999999999645 ) ) ;
#2408 = EDGE_CURVE ( 'NONE', #190, #2577, #1037, .T. ) ;
#2409 = ORIENTED_EDGE ( 'NONE', *, *, #2055, .F. ) ;
#2410 = CARTESIAN_POINT ( 'NONE',  ( 66.99999999999997158, -5.000000000000000000, -44.49999999999999289 ) ) ;
#2411 = EDGE_CURVE ( 'NONE', #2972, #448, #209, .T. ) ;
#2412 = ORIENTED_EDGE ( 'NONE', *, *, #1742, .F. ) ;
#2413 = CARTESIAN_POINT ( 'NONE',  ( -45.00000000000000000, 45.00000000000000711, -9.999999999999994671 ) ) ;
#2414 =( NAMED_UNIT ( * ) SI_UNIT ( $, .STERADIAN. ) SOLID_ANGLE_UNIT ( ) );
#2415 = CARTESIAN_POINT ( 'NONE',  ( -66.99999999999997158, -5.000000000000000000, 41.99999999999999289 ) ) ;
#2416 = CARTESIAN_POINT ( 'NONE',  ( -44.99999999999999289, 50.00000000000000000, 12.15000000000000391 ) ) ;
#2417 = EDGE_CURVE ( 'NONE', #2683, #699, #1765, .T. ) ;
#2418 = LINE ( 'NONE', #833, #2556 ) ;
#2419 = ORIENTED_EDGE ( 'NONE', *, *, #970, .T. ) ;
#2420 =( REPRESENTATION_RELATIONSHIP ('NONE','NONE', #3165, #1050 ) REPRESENTATION_RELATIONSHIP_WITH_TRANSFORMATION ( #3064 )SHAPE_REPRESENTATION_RELATIONSHIP( ) );
#2421 = ORIENTED_EDGE ( 'NONE', *, *, #815, .T. ) ;
#2422 = CARTESIAN_POINT ( 'NONE',  ( 4.000000000000003553, 0.000000000000000000, 3.500000000000000000 ) ) ;
#2423 = FACE_OUTER_BOUND ( 'NONE', #2936, .T. ) ;
#2424 = ORIENTED_EDGE ( 'NONE', *, *, #2624, .T. ) ;
#2425 = CARTESIAN_POINT ( 'NONE',  ( -7.250000000000000000, 25.00000000000000000, 47.00000000000000000 ) ) ;
#2426 = SURFACE_SIDE_STYLE ('',( #1071 ) ) ;
#2427 = EDGE_LOOP ( 'NONE', ( #306, #1067, #155, #3369, #2886, #3011 ) ) ;
#2428 = ADVANCED_FACE ( 'NONE', ( #1543 ), #2786, .T. ) ;
#2429 = CARTESIAN_POINT ( 'NONE',  ( 0.000000000000000000, 120.0000000000000142, 0.000000000000000000 ) ) ;
#2430 =( NAMED_UNIT ( * ) SI_UNIT ( $, .STERADIAN. ) SOLID_ANGLE_UNIT ( ) );
#2431 = CARTESIAN_POINT ( 'NONE',  ( -75.00000000000000000, 50.00000000000000000, 50.00000000000000000 ) ) ;
#2432 = LINE ( 'NONE', #96, #2717 ) ;
#2433 = CIRCLE ( 'NONE', #2760, 1.535500000000000087 ) ;
#2434 = DIRECTION ( 'NONE',  ( -0.000000000000000000, 1.000000000000000000, -0.000000000000000000 ) ) ;
#2435 = VERTEX_POINT ( 'NONE', #2803 ) ;
#2436 = EDGE_CURVE ( 'NONE', #22, #331, #484, .T. ) ;
#2437 = ORIENTED_EDGE ( 'NONE', *, *, #2696, .T. ) ;
#2438 = VECTOR ( 'NONE', #1379, 1000.000000000000000 ) ;
#2439 = FACE_OUTER_BOUND ( 'NONE', #2902, .T. ) ;
#2440=STYLED_ITEM('',(#3422),#573);
#2441 = FACE_OUTER_BOUND ( 'NONE', #451, .T. ) ;
#2442 = AXIS2_PLACEMENT_3D ( 'NONE', #1143, #3178, #2948 ) ;
#2443 = VECTOR ( 'NONE', #2492, 1000.000000000000000 ) ;
#2444 = ORIENTED_EDGE ( 'NONE', *, *, #409, .T. ) ;
#2445 = CARTESIAN_POINT ( 'NONE',  ( 4.200000000000001954, 0.000000000000000000, 2.000000000000000888 ) ) ;
#2446 = AXIS2_PLACEMENT_3D ( 'NONE', #2819, #3360, #3046 ) ;
#2447 = AXIS2_PLACEMENT_3D ( 'NONE', #924, #1232, #1200 ) ;
#2448 = SHAPE_DEFINITION_REPRESENTATION ( #3352, #936 ) ;
#2449 = CIRCLE ( 'NONE', #1085, 7.250000000000000000 ) ;
#2450 = ORIENTED_EDGE ( 'NONE', *, *, #2436, .F. ) ;
#2451 = LINE ( 'NONE', #115, #1841 ) ;
#2452 = VECTOR ( 'NONE', #1267, 1000.000000000000000 ) ;
#2453 = ADVANCED_FACE ( 'NONE', ( #1490 ), #453, .T. ) ;
#2454 =( NAMED_UNIT ( * ) PLANE_ANGLE_UNIT ( ) SI_UNIT ( $, .RADIAN. ) );
#2455 =( GEOMETRIC_REPRESENTATION_CONTEXT ( 3 ) GLOBAL_UNCERTAINTY_ASSIGNED_CONTEXT ( ( #615 ) ) GLOBAL_UNIT_ASSIGNED_CONTEXT ( ( #1164, #2773, #2843 ) ) REPRESENTATION_CONTEXT ( 'NONE', 'WORKASPACE' ) );
#2456 = SURFACE_STYLE_FILL_AREA ( #2776 ) ;
#2457 = DIRECTION ( 'NONE',  ( 1.000000000000000000, 0.000000000000000000, 0.000000000000000000 ) ) ;
#2458 = ADVANCED_FACE ( 'NONE', ( #2311 ), #2856, .F. ) ;
#2459 = CARTESIAN_POINT ( 'NONE',  ( 0.000000000000000000, 52.00000000000000711, 0.000000000000000000 ) ) ;
#2460 = VERTEX_POINT ( 'NONE', #191 ) ;
#2461 = CARTESIAN_POINT ( 'NONE',  ( 55.00000000000000000, 120.0000000000000142, -5.000000000000000000 ) ) ;
#2462 = DIRECTION ( 'NONE',  ( 0.000000000000000000, -1.000000000000000000, 0.000000000000000000 ) ) ;
#2463 = FACE_OUTER_BOUND ( 'NONE', #1522, .T. ) ;
#2464 = VERTEX_POINT ( 'NONE', #2527 ) ;
#2465 = DIRECTION ( 'NONE',  ( 0.000000000000000000, 0.000000000000000000, 1.000000000000000000 ) ) ;
#2466 = PRODUCT_DEFINITION_CONTEXT ( 'detailed design', #1678, 'design' ) ;
#2467 = ADVANCED_FACE ( 'NONE', ( #2570 ), #2841, .F. ) ;
#2468 = APPLICATION_PROTOCOL_DEFINITION ( 'draft international standard', 'automotive_design', 1998, #2966 ) ;
#2469 = ORIENTED_EDGE ( 'NONE', *, *, #195, .T. ) ;
#2470 = FACE_OUTER_BOUND ( 'NONE', #1396, .T. ) ;
#2471 = CARTESIAN_POINT ( 'NONE',  ( -39.00000000000000000, 136.9705627484771355, 6.000000000000004441 ) ) ;
#2472 = CARTESIAN_POINT ( 'NONE',  ( 0.000000000000000000, 25.00000000000000000, 50.00000000000000000 ) ) ;
#2473 = LINE ( 'NONE', #457, #271 ) ;
#2474 = PLANE ( 'NONE',  #2322 ) ;
#2475 = EDGE_CURVE ( 'NONE', #3078, #499, #1300, .T. ) ;
#2476 = CARTESIAN_POINT ( 'NONE',  ( -45.00000000000000000, 50.00000000000000000, -11.99999999999999645 ) ) ;
#2477 = CARTESIAN_POINT ( 'NONE',  ( 45.00000000000000000, 45.00000000000000711, 9.999999999999994671 ) ) ;
#2478 = VERTEX_POINT ( 'NONE', #227 ) ;
#2479 = FACE_OUTER_BOUND ( 'NONE', #2139, .T. ) ;
#2480 = DIRECTION ( 'NONE',  ( 0.000000000000000000, 0.000000000000000000, 1.000000000000000000 ) ) ;
#2481 = ORIENTED_EDGE ( 'NONE', *, *, #891, .T. ) ;
#2482 = EDGE_CURVE ( 'NONE', #699, #2273, #3096, .T. ) ;
#2483 = DIRECTION ( 'NONE',  ( -0.000000000000000000, 1.000000000000000000, -0.000000000000000000 ) ) ;
#2484 = CARTESIAN_POINT ( 'NONE',  ( 7.500000000000000000, 25.00000000000000000, 47.00000000000000000 ) ) ;
#2485 = CARTESIAN_POINT ( 'NONE',  ( 7.500000000000000000, 25.00000000000000000, 47.00000000000000000 ) ) ;
#2486 = LINE ( 'NONE', #196, #164 ) ;
#2487 = CARTESIAN_POINT ( 'NONE',  ( 2.000000000000000000, 0.000000000000000000, 0.000000000000000000 ) ) ;
#2488 = CARTESIAN_POINT ( 'NONE',  ( 2.000000000000000000, 1.773042676681340524, -2.059984127722458425E-15 ) ) ;
#2489 = ADVANCED_FACE ( 'NONE', ( #2274 ), #779, .T. ) ;
#2490 = AXIS2_PLACEMENT_3D ( 'NONE', #421, #645, #1720 ) ;
#2491 = ORIENTED_EDGE ( 'NONE', *, *, #2334, .T. ) ;
#2492 = DIRECTION ( 'NONE',  ( -0.000000000000000000, 1.000000000000000000, -0.000000000000000000 ) ) ;
#2493 = UNCERTAINTY_MEASURE_WITH_UNIT (LENGTH_MEASURE( 1.000000000000000082E-05 ), #1560, 'distance_accuracy_value', 'NONE');
#2494 = VECTOR ( 'NONE', #1441, 1000.000000000000000 ) ;
#2495 = DIRECTION ( 'NONE',  ( 0.000000000000000000, 0.000000000000000000, -1.000000000000000000 ) ) ;
#2496 = ORIENTED_EDGE ( 'NONE', *, *, #60, .F. ) ;
#2497 = AXIS2_PLACEMENT_3D ( 'NONE', #627, #380, #1879 ) ;
#2498 = AXIS2_PLACEMENT_3D ( 'NONE', #359, #2207, #1402 ) ;
#2499 = CARTESIAN_POINT ( 'NONE',  ( 10.00000000000000178, 0.000000000000000000, 0.000000000000000000 ) ) ;
#2500 = AXIS2_PLACEMENT_3D ( 'NONE', #2940, #598, #1643 ) ;
#2501 = VECTOR ( 'NONE', #563, 1000.000000000000000 ) ;
#2502 = CARTESIAN_POINT ( 'NONE',  ( -49.99999999999999289, 52.00000000000000711, -4.999999999999996447 ) ) ;
#2503=STYLED_ITEM('',(#3408),#2945);
#2504 = FACE_OUTER_BOUND ( 'NONE', #3305, .T. ) ;
#2505 = CARTESIAN_POINT ( 'NONE',  ( 0.000000000000000000, 0.000000000000000000, 0.000000000000000000 ) ) ;
#2506 = DIRECTION ( 'NONE',  ( -1.000000000000000000, 0.000000000000000000, 0.000000000000000000 ) ) ;
#2507 = MECHANICAL_DESIGN_GEOMETRIC_PRESENTATION_REPRESENTATION (  '', ( #1313 ), #2455 ) ;
#2508 = LINE ( 'NONE', #3059, #1039 ) ;
#2509 = ORIENTED_EDGE ( 'NONE', *, *, #708, .T. ) ;
#2510 = LINE ( 'NONE', #2733, #2659 ) ;
#2511 = ADVANCED_FACE ( 'NONE', ( #3306 ), #963, .F. ) ;
#2512 = APPLICATION_PROTOCOL_DEFINITION ( 'draft international standard', 'automotive_design', 1998, #916 ) ;
#2513 = ORIENTED_EDGE ( 'NONE', *, *, #288, .T. ) ;
#2514 = EDGE_CURVE ( 'NONE', #35, #1538, #1324, .T. ) ;
#2515 = DIRECTION ( 'NONE',  ( 0.000000000000000000, 0.8660254037844380415, -0.5000000000000012212 ) ) ;
#2516 = ORIENTED_EDGE ( 'NONE', *, *, #1721, .F. ) ;
#2517 = CYLINDRICAL_SURFACE ( 'NONE', #2113, 2.000000000000000888 ) ;
#2518 = DIRECTION ( 'NONE',  ( 0.000000000000000000, 0.000000000000000000, -1.000000000000000000 ) ) ;
#2519 = CARTESIAN_POINT ( 'NONE',  ( -54.99999999999995026, 130.0000000000000000, 5.000000000000004441 ) ) ;
#2520 = DIRECTION ( 'NONE',  ( 0.000000000000000000, 0.000000000000000000, 1.000000000000000000 ) ) ;
#2521 = EDGE_CURVE ( 'NONE', #880, #940, #841, .T. ) ;
#2522 = PLANE ( 'NONE',  #2447 ) ;
#2523 = LINE ( 'NONE', #2236, #1524 ) ;
#2524 = ORIENTED_EDGE ( 'NONE', *, *, #611, .F. ) ;
#2525 = FACE_OUTER_BOUND ( 'NONE', #2563, .T. ) ;
#2526 = ORIENTED_EDGE ( 'NONE', *, *, #2482, .F. ) ;
#2527 = CARTESIAN_POINT ( 'NONE',  ( -54.99999999999995026, 120.0000000000000142, 5.000000000000004441 ) ) ;
#2528 = UNCERTAINTY_MEASURE_WITH_UNIT (LENGTH_MEASURE( 1.000000000000000082E-05 ), #1633, 'distance_accuracy_value', 'NONE');
#2529 = EDGE_CURVE ( 'NONE', #624, #740, #2379, .T. ) ;
#2530 = PRESENTATION_STYLE_ASSIGNMENT (( #2750 ) ) ;
#2531 = ORIENTED_EDGE ( 'NONE', *, *, #310, .T. ) ;
#2532 = DIRECTION ( 'NONE',  ( -0.000000000000000000, -0.000000000000000000, 1.000000000000000000 ) ) ;
#2533 = CARTESIAN_POINT ( 'NONE',  ( 2.000000000000000000, 1.773042676681340524, -2.059984127722458425E-15 ) ) ;
#2534 = PRESENTATION_STYLE_ASSIGNMENT (( #3053 ) ) ;
#2535 = LINE ( 'NONE', #2355, #2109 ) ;
#2536 = CARTESIAN_POINT ( 'NONE',  ( 2.000000000000000000, -1.773042676681341856, 2.276824562219559311E-15 ) ) ;
#2537 = DIRECTION ( 'NONE',  ( 0.000000000000000000, -0.000000000000000000, -1.000000000000000000 ) ) ;
#2538 = ADVANCED_FACE ( 'NONE', ( #3151 ), #2104, .F. ) ;
#2539 = EDGE_LOOP ( 'NONE', ( #3060, #1775, #1648, #1427 ) ) ;
#2540 = ORIENTED_EDGE ( 'NONE', *, *, #374, .T. ) ;
#2541 = CARTESIAN_POINT ( 'NONE',  ( 2.000000000000000000, 0.8865213383406680414, -1.535500000000000975 ) ) ;
#2542 = CIRCLE ( 'NONE', #1084, 4.500000000000010658 ) ;
#2543 = VERTEX_POINT ( 'NONE', #1866 ) ;
#2544 = AXIS2_PLACEMENT_3D ( 'NONE', #848, #1100, #590 ) ;
#2545 = FACE_BOUND ( 'NONE', #1592, .T. ) ;
#2546 = VECTOR ( 'NONE', #1493, 1000.000000000000000 ) ;
#2547 = CIRCLE ( 'NONE', #971, 2.149999999999999023 ) ;
#2548 = AXIS2_PLACEMENT_3D ( 'NONE', #1995, #3342, #1205 ) ;
#2549 = ORIENTED_EDGE ( 'NONE', *, *, #666, .F. ) ;
#2550 = CARTESIAN_POINT ( 'NONE',  ( -44.99999999999999289, 50.00000000000000000, 7.850000000000005862 ) ) ;
#2551 = PRODUCT ( 'Insulation Pad', 'Insulation Pad', '', ( #1967 ) ) ;
#2552 = EDGE_CURVE ( 'NONE', #1926, #223, #2363, .T. ) ;
#2553 = AXIS2_PLACEMENT_3D ( 'NONE', #1504, #2077, #1275 ) ;
#2554 = AXIS2_PLACEMENT_3D ( 'NONE', #597, #626, #2956 ) ;
#2555 = DIRECTION ( 'NONE',  ( 0.000000000000000000, 0.000000000000000000, -1.000000000000000000 ) ) ;
#2556 = VECTOR ( 'NONE', #2200, 1000.000000000000000 ) ;
#2557 = AXIS2_PLACEMENT_3D ( 'NONE', #3210, #1909, #2653 ) ;
#2558 = CARTESIAN_POINT ( 'NONE',  ( 44.99999999999999289, 50.00000000000000000, -8.000000000000003553 ) ) ;
#2559 = FACE_OUTER_BOUND ( 'NONE', #2202, .T. ) ;
#2560 = ADVANCED_FACE ( 'NONE', ( #11 ), #298, .T. ) ;
#2561 = LINE ( 'NONE', #20, #2884 ) ;
#2562 = ORIENTED_EDGE ( 'NONE', *, *, #3070, .F. ) ;
#2563 = EDGE_LOOP ( 'NONE', ( #214, #358, #313, #91 ) ) ;
#2564 = CARTESIAN_POINT ( 'NONE',  ( 2.000000000000000000, 0.000000000000000000, 1.535500000000000087 ) ) ;
#2565 = UNCERTAINTY_MEASURE_WITH_UNIT (LENGTH_MEASURE( 1.000000000000000082E-05 ), #567, 'distance_accuracy_value', 'NONE');
#2566 = AXIS2_PLACEMENT_3D ( 'NONE', #3304, #2480, #3256 ) ;
#2567 = CONTEXT_DEPENDENT_SHAPE_REPRESENTATION ( #2596, #2250 ) ;
#2568 = ORIENTED_EDGE ( 'NONE', *, *, #1885, .F. ) ;
#2569 = ADVANCED_FACE ( 'NONE', ( #311 ), #1595, .F. ) ;
#2570 = FACE_OUTER_BOUND ( 'NONE', #3145, .T. ) ;
#2571 = ORIENTED_EDGE ( 'NONE', *, *, #1712, .F. ) ;
#2572 = PLANE ( 'NONE',  #3278 ) ;
#2573 = PLANE ( 'NONE',  #40 ) ;
#2574 = CARTESIAN_POINT ( 'NONE',  ( -75.00000000000000000, 0.000000000000000000, 50.00000000000000000 ) ) ;
#2575 =( NAMED_UNIT ( * ) PLANE_ANGLE_UNIT ( ) SI_UNIT ( $, .RADIAN. ) );
#2576 = EDGE_CURVE ( 'NONE', #2115, #801, #792, .T. ) ;
#2577 = VERTEX_POINT ( 'NONE', #1089 ) ;
#2578 = ORIENTED_EDGE ( 'NONE', *, *, #1876, .T. ) ;
#2579 = CARTESIAN_POINT ( 'NONE',  ( -49.99999999999999289, 50.00000000000000000, -14.99999999999999645 ) ) ;
#2580 = ITEM_DEFINED_TRANSFORMATION ( 'NONE', 'NONE', #549,  #3111 ) ;
#2581 = EDGE_LOOP ( 'NONE', ( #3146, #547, #415, #2890 ) ) ;
#2582 = CARTESIAN_POINT ( 'NONE',  ( 0.000000000000000000, 25.00000000000000000, 47.00000000000000000 ) ) ;
#2583 = SURFACE_STYLE_FILL_AREA ( #2821 ) ;
#2584 = PRODUCT_DEFINITION ( 'UNKNOWN', '', #3229, #3288 ) ;
#2585 = VERTEX_POINT ( 'NONE', #1055 ) ;
#2586 = CARTESIAN_POINT ( 'NONE',  ( -66.99999999999997158, -5.000000000000000000, -44.49999999999999289 ) ) ;
#2587 = DIRECTION ( 'NONE',  ( -0.000000000000000000, 1.000000000000000000, -0.000000000000000000 ) ) ;
#2588 = DIRECTION ( 'NONE',  ( 0.000000000000000000, 0.000000000000000000, 1.000000000000000000 ) ) ;
#2589 = DIRECTION ( 'NONE',  ( -1.000000000000000000, 0.000000000000000000, 0.000000000000000000 ) ) ;
#2590 = DIRECTION ( 'NONE',  ( -1.000000000000000000, -0.000000000000000000, -0.000000000000000000 ) ) ;
#2591 = EDGE_LOOP ( 'NONE', ( #1640, #498, #1749, #345 ) ) ;
#2592 = ORIENTED_EDGE ( 'NONE', *, *, #159, .T. ) ;
#2593 = CARTESIAN_POINT ( 'NONE',  ( 2.000000000000000000, 1.773042676681340524, -2.059984127722458425E-15 ) ) ;
#2594 = AXIS2_PLACEMENT_3D ( 'NONE', #2264, #1199, #2520 ) ;
#2595 = EDGE_CURVE ( 'NONE', #113, #2761, #1964, .T. ) ;
#2596 =( REPRESENTATION_RELATIONSHIP ('NONE','NONE', #3165, #1050 ) REPRESENTATION_RELATIONSHIP_WITH_TRANSFORMATION ( #2580 )SHAPE_REPRESENTATION_RELATIONSHIP( ) );
#2597 = VERTEX_POINT ( 'NONE', #566 ) ;
#2598 = DIRECTION ( 'NONE',  ( 0.000000000000000000, -1.000000000000000000, 0.000000000000000000 ) ) ;
#2599 = EDGE_CURVE ( 'NONE', #3174, #3078, #3189, .T. ) ;
#2600 = ORIENTED_EDGE ( 'NONE', *, *, #1852, .T. ) ;
#2601 = AXIS2_PLACEMENT_3D ( 'NONE', #3193, #571, #2382 ) ;
#2602 = SURFACE_SIDE_STYLE ('',( #2456 ) ) ;
#2603 = VECTOR ( 'NONE', #336, 1000.000000000000000 ) ;
#2604 = VECTOR ( 'NONE', #1312, 1000.000000000000000 ) ;
#2605 = DIRECTION ( 'NONE',  ( 0.000000000000000000, -1.000000000000000000, 0.000000000000000000 ) ) ;
#2606 = CARTESIAN_POINT ( 'NONE',  ( 4.200000000000001954, 0.000000000000000000, 0.000000000000000000 ) ) ;
#2607 = AXIS2_PLACEMENT_3D ( 'NONE', #3316, #2267, #199 ) ;
#2608 = LINE ( 'NONE', #3366, #2284 ) ;
#2609 = VECTOR ( 'NONE', #1398, 1000.000000000000000 ) ;
#2610 = ADVANCED_FACE ( 'NONE', ( #2905 ), #826, .T. ) ;
#2611 = PRODUCT_DEFINITION_SHAPE ( 'NONE', 'NONE',  #273 ) ;
#2612 = DIRECTION ( 'NONE',  ( -0.000000000000000000, -1.000000000000000000, -0.000000000000000000 ) ) ;
#2613 = AXIS2_PLACEMENT_3D ( 'NONE', #1343, #2915, #2675 ) ;
#2614 = ORIENTED_EDGE ( 'NONE', *, *, #1701, .T. ) ;
#2615 = ORIENTED_EDGE ( 'NONE', *, *, #2334, .F. ) ;
#2616 = CARTESIAN_POINT ( 'NONE',  ( -66.99999999999997158, -6.000000000000000000, 41.99999999999999289 ) ) ;
#2617 = AXIS2_PLACEMENT_3D ( 'NONE', #132, #420, #1462 ) ;
#2618 =( GEOMETRIC_REPRESENTATION_CONTEXT ( 3 ) GLOBAL_UNCERTAINTY_ASSIGNED_CONTEXT ( ( #1472 ) ) GLOBAL_UNIT_ASSIGNED_CONTEXT ( ( #1056, #3345, #228 ) ) REPRESENTATION_CONTEXT ( 'NONE', 'WORKASPACE' ) );
#2619 = ORIENTED_EDGE ( 'NONE', *, *, #2755, .T. ) ;
#2620 = CARTESIAN_POINT ( 'NONE',  ( 75.00000000000000000, 50.00000000000000000, 50.00000000000000000 ) ) ;
#2621 = AXIS2_PLACEMENT_3D ( 'NONE', #2622, #1325, #2364 ) ;
#2622 = CARTESIAN_POINT ( 'NONE',  ( 0.000000000000000000, 0.000000000000000000, 0.000000000000000000 ) ) ;
#2623 = VERTEX_POINT ( 'NONE', #1916 ) ;
#2624 = EDGE_CURVE ( 'NONE', #1054, #1203, #1673, .T. ) ;
#2625 = LINE ( 'NONE', #286, #369 ) ;
#2626 = FACE_OUTER_BOUND ( 'NONE', #905, .T. ) ;
#2627 = DIRECTION ( 'NONE',  ( 0.000000000000000000, 0.000000000000000000, -1.000000000000000000 ) ) ;
#2628 = LINE ( 'NONE', #1550, #749 ) ;
#2629 = CARTESIAN_POINT ( 'NONE',  ( 0.1999999999999987899, 0.000000000000000000, 3.299999999999999822 ) ) ;
#2630 = ORIENTED_EDGE ( 'NONE', *, *, #2911, .F. ) ;
#2631 = ADVANCED_FACE ( 'NONE', ( #123 ), #330, .F. ) ;
#2632 = EDGE_LOOP ( 'NONE', ( #34, #1733, #281, #2694 ) ) ;
#2633 = DIRECTION ( 'NONE',  ( 0.000000000000000000, 0.000000000000000000, 1.000000000000000000 ) ) ;
#2634 = ORIENTED_EDGE ( 'NONE', *, *, #106, .T. ) ;
#2635 = CARTESIAN_POINT ( 'NONE',  ( -44.99999999999999289, 52.00000000000000711, 10.00000000000000533 ) ) ;
#2636 = EDGE_LOOP ( 'NONE', ( #3131, #1113 ) ) ;
#2637 = DIRECTION ( 'NONE',  ( 0.000000000000000000, 0.000000000000000000, 1.000000000000000000 ) ) ;
#2638 = ADVANCED_FACE ( 'NONE', ( #854 ), #1930, .F. ) ;
#2639 = DIRECTION ( 'NONE',  ( 1.000000000000000000, 0.000000000000000000, 0.000000000000000000 ) ) ;
#2640 = CARTESIAN_POINT ( 'NONE',  ( -39.99999999999999289, 50.00000000000000000, 15.00000000000000178 ) ) ;
#2641 = DIRECTION ( 'NONE',  ( -6.938893903907228378E-16, -0.000000000000000000, 1.000000000000000000 ) ) ;
#2642 = DIRECTION ( 'NONE',  ( -1.000000000000000000, -0.000000000000000000, -0.000000000000000000 ) ) ;
#2643 = VERTEX_POINT ( 'NONE', #1621 ) ;
#2644 = EDGE_LOOP ( 'NONE', ( #2744, #3290, #1209, #525 ) ) ;
#2645 = CARTESIAN_POINT ( 'NONE',  ( -49.99999999999999289, 50.00000000000000000, -14.99999999999999645 ) ) ;
#2646 = ORIENTED_EDGE ( 'NONE', *, *, #1596, .T. ) ;
#2647 = DIRECTION ( 'NONE',  ( 0.000000000000000000, 0.000000000000000000, 1.000000000000000000 ) ) ;
#2648 = DIRECTION ( 'NONE',  ( 1.000000000000000000, 0.000000000000000000, 0.000000000000000000 ) ) ;
#2649 = ORIENTED_EDGE ( 'NONE', *, *, #2143, .F. ) ;
#2650 = DIRECTION ( 'NONE',  ( 1.000000000000000000, 0.000000000000000000, 0.000000000000000000 ) ) ;
#2651 = CARTESIAN_POINT ( 'NONE',  ( -66.99999999999997158, -8.000000000000000000, 48.00000000000000000 ) ) ;
#2652 = EDGE_CURVE ( 'NONE', #1319, #1875, #2226, .T. ) ;
#2653 = DIRECTION ( 'NONE',  ( 0.000000000000000000, 0.000000000000000000, 1.000000000000000000 ) ) ;
#2654 = CIRCLE ( 'NONE', #1511, 2.149999999999999023 ) ;
#2655 = AXIS2_PLACEMENT_3D ( 'NONE', #1872, #2913, #1392 ) ;
#2656 = DIRECTION ( 'NONE',  ( -1.387778780781445676E-16, -0.000000000000000000, 1.000000000000000000 ) ) ;
#2657 = ORIENTED_EDGE ( 'NONE', *, *, #2685, .F. ) ;
#2658 = AXIS2_PLACEMENT_3D ( 'NONE', #3104, #2299, #2279 ) ;
#2659 = VECTOR ( 'NONE', #3062, 1000.000000000000000 ) ;
#2660 = ORIENTED_EDGE ( 'NONE', *, *, #3144, .F. ) ;
#2661 = ADVANCED_FACE ( 'NONE', ( #2463, #3253 ), #578, .F. ) ;
#2662 = DIRECTION ( 'NONE',  ( 1.000000000000000000, 0.000000000000000000, -6.938893903907232322E-16 ) ) ;
#2663 = AXIS2_PLACEMENT_3D ( 'NONE', #3080, #737, #1800 ) ;
#2664 = AXIS2_PLACEMENT_3D ( 'NONE', #2065, #2302, #2084 ) ;
#2665 = CARTESIAN_POINT ( 'NONE',  ( -66.99999999999997158, 0.000000000000000000, -44.49999999999999289 ) ) ;
#2666 = EDGE_LOOP ( 'NONE', ( #3050, #1065, #1385, #2513 ) ) ;
#2667 = VECTOR ( 'NONE', #2982, 1000.000000000000000 ) ;
#2668 = DIRECTION ( 'NONE',  ( 1.000000000000000000, 0.000000000000000000, 0.000000000000000000 ) ) ;
#2669 = FILL_AREA_STYLE ('',( #601 ) ) ;
#2670 = EDGE_LOOP ( 'NONE', ( #1001, #1124, #398, #2390 ) ) ;
#2671 = ADVANCED_FACE ( 'NONE', ( #2191 ), #697, .F. ) ;
#2672 = DIRECTION ( 'NONE',  ( -1.000000000000000000, 0.000000000000000000, 0.000000000000000000 ) ) ;
#2673 = DIRECTION ( 'NONE',  ( -0.000000000000000000, 1.000000000000000000, -0.000000000000000000 ) ) ;
#2674 = LINE ( 'NONE', #338, #1622 ) ;
#2675 = DIRECTION ( 'NONE',  ( 0.000000000000000000, 0.000000000000000000, -1.000000000000000000 ) ) ;
#2676 = ORIENTED_EDGE ( 'NONE', *, *, #2943, .T. ) ;
#2677 = ORIENTED_EDGE ( 'NONE', *, *, #2576, .F. ) ;
#2678 = CARTESIAN_POINT ( 'NONE',  ( 0.000000000000000000, 0.000000000000000000, 0.000000000000000000 ) ) ;
#2679 = ADVANCED_FACE ( 'NONE', ( #904 ), #1941, .T. ) ;
#2680 = LINE ( 'NONE', #344, #810 ) ;
#2681 = ORIENTED_EDGE ( 'NONE', *, *, #2219, .F. ) ;
#2682 = CARTESIAN_POINT ( 'NONE',  ( -75.00000000000000000, 0.000000000000000000, 50.00000000000000000 ) ) ;
#2683 = VERTEX_POINT ( 'NONE', #1123 ) ;
#2684 = CARTESIAN_POINT ( 'NONE',  ( 0.000000000000000000, -0.8865213383406694847, 1.535500000000001419 ) ) ;
#2685 = EDGE_CURVE ( 'NONE', #2003, #2103, #589, .T. ) ;
#2686 = FILL_AREA_STYLE ('',( #2147 ) ) ;
#2687 = DIRECTION ( 'NONE',  ( 0.000000000000000000, 0.000000000000000000, 1.000000000000000000 ) ) ;
#2688 = LINE ( 'NONE', #1924, #2126 ) ;
#2689 = DIRECTION ( 'NONE',  ( 0.000000000000000000, 0.000000000000000000, 1.000000000000000000 ) ) ;
#2690 = ORIENTED_EDGE ( 'NONE', *, *, #619, .F. ) ;
#2691 = VERTEX_POINT ( 'NONE', #2665 ) ;
#2692 = FACE_BOUND ( 'NONE', #2049, .T. ) ;
#2693 = DIRECTION ( 'NONE',  ( 1.000000000000000000, 0.000000000000000000, 0.000000000000000000 ) ) ;
#2694 = ORIENTED_EDGE ( 'NONE', *, *, #3024, .F. ) ;
#2695 = CARTESIAN_POINT ( 'NONE',  ( -31.74999999999995737, 4.286263797015736595E-16, -3.500000000000000000 ) ) ;
#2696 = EDGE_CURVE ( 'NONE', #2976, #468, #2280, .T. ) ;
#2697 = EDGE_LOOP ( 'NONE', ( #2961, #599, #3130, #2813, #2373 ) ) ;
#2698 = ADVANCED_FACE ( 'NONE', ( #2141 ), #1893, .T. ) ;
#2699 = DIRECTION ( 'NONE',  ( 0.000000000000000000, 0.5000000000000011102, 0.8660254037844379305 ) ) ;
#2700 = CLOSED_SHELL ( 'NONE', ( #3176, #2467, #2963, #2929, #168, #3292, #1014, #596, #1171, #2791 ) ) ;
#2701 = DIRECTION ( 'NONE',  ( -0.000000000000000000, -1.000000000000000000, -0.000000000000000000 ) ) ;
#2702 = DIRECTION ( 'NONE',  ( -0.000000000000000000, -1.000000000000000000, -0.000000000000000000 ) ) ;
#2703 = LINE ( 'NONE', #607, #3047 ) ;
#2704 = EDGE_LOOP ( 'NONE', ( #429, #2531, #1639 ) ) ;
#2705 = DIRECTION ( 'NONE',  ( -0.000000000000000000, 0.000000000000000000, 1.000000000000000000 ) ) ;
#2706 = AXIS2_PLACEMENT_3D ( 'NONE', #2951, #832, #1873 ) ;
#2707 = ADVANCED_FACE ( 'NONE', ( #837 ), #3200, .F. ) ;
#2708 = CARTESIAN_POINT ( 'NONE',  ( 0.000000000000000000, 25.00000000000000000, 47.00000000000000000 ) ) ;
#2709 = DIRECTION ( 'NONE',  ( -0.000000000000000000, 1.000000000000000000, -0.000000000000000000 ) ) ;
#2710 = VECTOR ( 'NONE', #2093, 1000.000000000000000 ) ;
#2711 = ORIENTED_EDGE ( 'NONE', *, *, #2863, .F. ) ;
#2712 = CARTESIAN_POINT ( 'NONE',  ( -74.99999999999998579, 50.00000000000000000, -50.00000000000000000 ) ) ;
#2713 = AXIS2_PLACEMENT_3D ( 'NONE', #1993, #3035, #2216 ) ;
#2714 = VECTOR ( 'NONE', #2729, 1000.000000000000000 ) ;
#2715 =( LENGTH_UNIT ( ) NAMED_UNIT ( * ) SI_UNIT ( .MILLI., .METRE. ) );
#2716 = AXIS2_PLACEMENT_3D ( 'NONE', #2629, #2357, #2318 ) ;
#2717 = VECTOR ( 'NONE', #2185, 1000.000000000000000 ) ;
#2718 = ORIENTED_EDGE ( 'NONE', *, *, #646, .T. ) ;
#2719 = DIRECTION ( 'NONE',  ( -0.000000000000000000, -1.000000000000000000, -0.000000000000000000 ) ) ;
#2720 = EDGE_CURVE ( 'NONE', #2222, #3236, #2680, .T. ) ;
#2721 = FILL_AREA_STYLE_COLOUR ( '', #769 ) ;
#2722 =( GEOMETRIC_REPRESENTATION_CONTEXT ( 3 ) GLOBAL_UNCERTAINTY_ASSIGNED_CONTEXT ( ( #3120 ) ) GLOBAL_UNIT_ASSIGNED_CONTEXT ( ( #897, #439, #1702 ) ) REPRESENTATION_CONTEXT ( 'NONE', 'WORKASPACE' ) );
#2723 = PLANE ( 'NONE',  #2986 ) ;
#2724 = DIRECTION ( 'NONE',  ( -0.000000000000000000, 1.000000000000000000, -0.000000000000000000 ) ) ;
#2725 = APPLICATION_CONTEXT ( 'automotive_design' ) ;
#2726 = AXIS2_PLACEMENT_3D ( 'NONE', #1662, #2495, #1996 ) ;
#2727 = LINE ( 'NONE', #407, #1741 ) ;
#2728 = ORIENTED_EDGE ( 'NONE', *, *, #2101, .F. ) ;
#2729 = DIRECTION ( 'NONE',  ( 0.000000000000000000, 0.000000000000000000, -1.000000000000000000 ) ) ;
#2730 = CARTESIAN_POINT ( 'NONE',  ( 44.99999999999999289, 50.00000000000000000, -10.00000000000000533 ) ) ;
#2731 = ADVANCED_FACE ( 'NONE', ( #2423 ), #3216, .F. ) ;
#2732 = VERTEX_POINT ( 'NONE', #1658 ) ;
#2733 = CARTESIAN_POINT ( 'NONE',  ( -49.99999999999999289, 52.00000000000000711, -4.999999999999995559 ) ) ;
#2734 = ORIENTED_EDGE ( 'NONE', *, *, #1876, .F. ) ;
#2735 = DIRECTION ( 'NONE',  ( 0.000000000000000000, -0.5000000000000011102, -0.8660254037844379305 ) ) ;
#2736 = LINE ( 'NONE', #405, #1838 ) ;
#2737 = CYLINDRICAL_SURFACE ( 'NONE', #1190, 2.000000000000001776 ) ;
#2738 = ADVANCED_FACE ( 'NONE', ( #357, #2441 ), #105, .F. ) ;
#2739 =( NAMED_UNIT ( * ) PLANE_ANGLE_UNIT ( ) SI_UNIT ( $, .RADIAN. ) );
#2740 = LINE ( 'NONE', #1693, #3087 ) ;
#2741 = LINE ( 'NONE', #1181, #2714 ) ;
#2742 = SURFACE_STYLE_FILL_AREA ( #926 ) ;
#2743 = ORIENTED_EDGE ( 'NONE', *, *, #1489, .T. ) ;
#2744 = ORIENTED_EDGE ( 'NONE', *, *, #2920, .F. ) ;
#2745 = FACE_OUTER_BOUND ( 'NONE', #1152, .T. ) ;
#2746 =( REPRESENTATION_RELATIONSHIP ('NONE','NONE', #3165, #1286 ) REPRESENTATION_RELATIONSHIP_WITH_TRANSFORMATION ( #3358 )SHAPE_REPRESENTATION_RELATIONSHIP( ) );
#2747 = APPLICATION_PROTOCOL_DEFINITION ( 'draft international standard', 'automotive_design', 1998, #396 ) ;
#2748 = ORIENTED_EDGE ( 'NONE', *, *, #2755, .F. ) ;
#2749 = DIRECTION ( 'NONE',  ( 0.000000000000000000, -1.000000000000000000, 0.000000000000000000 ) ) ;
#2750 = SURFACE_STYLE_USAGE ( .BOTH. , #1971 ) ;
#2751 = FACE_OUTER_BOUND ( 'NONE', #602, .T. ) ;
#2752 = CARTESIAN_POINT ( 'NONE',  ( 45.00000000000000000, 50.00000000000000000, 9.999999999999994671 ) ) ;
#2753 = CLOSED_SHELL ( 'NONE', ( #452, #236, #3173, #2371, #1754, #3244 ) ) ;
#2754 = CARTESIAN_POINT ( 'NONE',  ( 45.00000000000000000, 50.00000000000000000, 11.99999999999999645 ) ) ;
#2755 = EDGE_CURVE ( 'NONE', #887, #21, #2768, .T. ) ;
#2756 = ORIENTED_EDGE ( 'NONE', *, *, #3206, .T. ) ;
#2757 = DIRECTION ( 'NONE',  ( -1.000000000000000000, 0.000000000000000000, -0.000000000000000000 ) ) ;
#2758 = DIRECTION ( 'NONE',  ( 0.000000000000000000, -1.000000000000000000, 0.000000000000000000 ) ) ;
#2759 = ADVANCED_FACE ( 'NONE', ( #1518 ), #1202, .F. ) ;
#2760 = AXIS2_PLACEMENT_3D ( 'NONE', #2487, #1466, #1231 ) ;
#2761 = VERTEX_POINT ( 'NONE', #1183 ) ;
#2762 = DIRECTION ( 'NONE',  ( -0.000000000000000000, 1.000000000000000000, -0.000000000000000000 ) ) ;
#2763 = AXIS2_PLACEMENT_3D ( 'NONE', #1969, #1715, #2241 ) ;
#2764 = CARTESIAN_POINT ( 'NONE',  ( -45.00000000000000000, 56.00000000000000711, -9.999999999999994671 ) ) ;
#2765 = PRODUCT_DEFINITION_SHAPE ( 'NONE', 'NONE',  #3380 ) ;
#2766 = EDGE_LOOP ( 'NONE', ( #3061, #2649 ) ) ;
#2767 =( REPRESENTATION_RELATIONSHIP ('NONE','NONE', #3165, #2804 ) REPRESENTATION_RELATIONSHIP_WITH_TRANSFORMATION ( #1012 )SHAPE_REPRESENTATION_RELATIONSHIP( ) );
#2768 = CIRCLE ( 'NONE', #2607, 2.200000000000001066 ) ;
#2769 = CIRCLE ( 'NONE', #695, 2.499999999999995115 ) ;
#2770 = DIRECTION ( 'NONE',  ( 0.000000000000000000, 0.000000000000000000, 1.000000000000000000 ) ) ;
#2771 =( GEOMETRIC_REPRESENTATION_CONTEXT ( 3 ) GLOBAL_UNCERTAINTY_ASSIGNED_CONTEXT ( ( #77 ) ) GLOBAL_UNIT_ASSIGNED_CONTEXT ( ( #1447, #678, #426 ) ) REPRESENTATION_CONTEXT ( 'NONE', 'WORKASPACE' ) );
#2772 = AXIS2_PLACEMENT_3D ( 'NONE', #234, #3351, #2287 ) ;
#2773 =( NAMED_UNIT ( * ) PLANE_ANGLE_UNIT ( ) SI_UNIT ( $, .RADIAN. ) );
#2774 = EDGE_CURVE ( 'NONE', #2775, #617, #1575, .T. ) ;
#2775 = VERTEX_POINT ( 'NONE', #974 ) ;
#2776 = FILL_AREA_STYLE ('',( #687 ) ) ;
#2777 = LINE ( 'NONE', #2485, #213 ) ;
#2778 = CARTESIAN_POINT ( 'NONE',  ( -66.99999999999997158, -6.000000000000000000, 41.99999999999999289 ) ) ;
#2779 =( GEOMETRIC_REPRESENTATION_CONTEXT ( 3 ) GLOBAL_UNCERTAINTY_ASSIGNED_CONTEXT ( ( #2293 ) ) GLOBAL_UNIT_ASSIGNED_CONTEXT ( ( #911, #1189, #3014 ) ) REPRESENTATION_CONTEXT ( 'NONE', 'WORKASPACE' ) );
#2780 = DIRECTION ( 'NONE',  ( -1.000000000000000000, 0.000000000000000000, -0.000000000000000000 ) ) ;
#2781 = DIRECTION ( 'NONE',  ( 0.000000000000000000, 0.000000000000000000, -1.000000000000000000 ) ) ;
#2782 = ORIENTED_EDGE ( 'NONE', *, *, #898, .F. ) ;
#2783 = LINE ( 'NONE', #1966, #2066 ) ;
#2784 = EDGE_CURVE ( 'NONE', #895, #3174, #1252, .T. ) ;
#2785 = ORIENTED_EDGE ( 'NONE', *, *, #1250, .T. ) ;
#2786 = CYLINDRICAL_SURFACE ( 'NONE', #2553, 2.499999999999995115 ) ;
#2787 = APPLICATION_PROTOCOL_DEFINITION ( 'draft international standard', 'automotive_design', 1998, #2377 ) ;
#2788 = EDGE_LOOP ( 'NONE', ( #748, #2996, #1104, #1943 ) ) ;
#2789 = CARTESIAN_POINT ( 'NONE',  ( 55.00000000000004974, 120.0000000000000142, 5.000000000000004441 ) ) ;
#2790 = LINE ( 'NONE', #656, #1403 ) ;
#2791 = ADVANCED_FACE ( 'NONE', ( #2014 ), #1723, .T. ) ;
#2792 = MANIFOLD_SOLID_BREP ( 'AdvancedHole1', #1828 ) ;
#2793 = SURFACE_STYLE_FILL_AREA ( #1443 ) ;
#2794 = DIRECTION ( 'NONE',  ( 0.000000000000000000, 0.000000000000000000, -1.000000000000000000 ) ) ;
#2795 = DIRECTION ( 'NONE',  ( 0.000000000000000000, -1.000000000000000000, 1.345283343056720273E-15 ) ) ;
#2796 = PRODUCT ( 'socket head cap screw_iso_ISO 4762 M4 x 6 - 6N', 'socket head cap screw_iso_ISO 4762 M4 x 6 - 6N', '', ( #401 ) ) ;
#2797 = SURFACE_SIDE_STYLE ('',( #2251 ) ) ;
#2798 = ORIENTED_EDGE ( 'NONE', *, *, #1134, .F. ) ;
#2799 = EDGE_LOOP ( 'NONE', ( #835, #3332, #376, #564 ) ) ;
#2800 = LINE ( 'NONE', #1501, #1195 ) ;
#2801 = ORIENTED_EDGE ( 'NONE', *, *, #325, .T. ) ;
#2802 = EDGE_CURVE ( 'NONE', #2086, #2115, #2523, .T. ) ;
#2803 = CARTESIAN_POINT ( 'NONE',  ( 2.000000000000000000, 0.8865213383406715941, 1.535499999999999199 ) ) ;
#2804 = SHAPE_REPRESENTATION ( 'Insulation Pad', ( #3111 ), #2889 ) ;
#2805 = ORIENTED_EDGE ( 'NONE', *, *, #907, .T. ) ;
#2806 = EDGE_CURVE ( 'NONE', #347, #2115, #2125, .T. ) ;
#2807 = CARTESIAN_POINT ( 'NONE',  ( 55.00000000000004974, 130.0000000000000000, 5.000000000000004441 ) ) ;
#2808 = DIRECTION ( 'NONE',  ( 0.000000000000000000, 0.000000000000000000, 1.000000000000000000 ) ) ;
#2809 = CARTESIAN_POINT ( 'NONE',  ( -40.00000000000000000, 117.0000000000000000, -4.999999999999995559 ) ) ;
#2810 = SURFACE_STYLE_USAGE ( .BOTH. , #2033 ) ;
#2811 = ORIENTED_EDGE ( 'NONE', *, *, #2211, .T. ) ;
#2812 = EDGE_CURVE ( 'NONE', #2732, #2239, #2508, .T. ) ;
#2813 = ORIENTED_EDGE ( 'NONE', *, *, #658, .T. ) ;
#2814 = CARTESIAN_POINT ( 'NONE',  ( -40.00000000000000000, 120.0000000000000142, 5.000000000000004441 ) ) ;
#2815 = VECTOR ( 'NONE', #522, 1000.000000000000114 ) ;
#2816 = SHAPE_DEFINITION_REPRESENTATION ( #1459, #685 ) ;
#2817 = ORIENTED_EDGE ( 'NONE', *, *, #1626, .F. ) ;
#2818 = VECTOR ( 'NONE', #2136, 999.9999999999998863 ) ;
#2819 = CARTESIAN_POINT ( 'NONE',  ( -66.99999999999997158, 0.000000000000000000, 41.99999999999999289 ) ) ;
#2820 = MANIFOLD_SOLID_BREP ( 'M4 Clearance Hole1', #3367 ) ;
#2821 = FILL_AREA_STYLE ('',( #12 ) ) ;
#2822 = CONICAL_SURFACE ( 'NONE', #2442, 1.535500000000000087, 1.047197551196590748 ) ;
#2823 = AXIS2_PLACEMENT_3D ( 'NONE', #2307, #776, #2835 ) ;
#2824 = ORIENTED_EDGE ( 'NONE', *, *, #259, .F. ) ;
#2825 = DIRECTION ( 'NONE',  ( 0.000000000000000000, -1.000000000000000000, 0.000000000000000000 ) ) ;
#2826 = AXIS2_PLACEMENT_3D ( 'NONE', #2407, #1383, #2153 ) ;
#2827 = EDGE_CURVE ( 'NONE', #2855, #2103, #1978, .T. ) ;
#2828 = FACE_OUTER_BOUND ( 'NONE', #877, .T. ) ;
#2829 = AXIS2_PLACEMENT_3D ( 'NONE', #773, #2304, #3112 ) ;
#2830 = PLANE ( 'NONE',  #1294 ) ;
#2831 = DIRECTION ( 'NONE',  ( -0.000000000000000000, 1.000000000000000000, -0.000000000000000000 ) ) ;
#2832 = PRESENTATION_LAYER_ASSIGNMENT (  '', '', ( #1468 ) ) ;
#2833 = VERTEX_POINT ( 'NONE', #253 ) ;
#2834 = VERTEX_POINT ( 'NONE', #1537 ) ;
#2835 = DIRECTION ( 'NONE',  ( 0.000000000000000000, 0.000000000000000000, -1.000000000000000000 ) ) ;
#2836 = UNCERTAINTY_MEASURE_WITH_UNIT (LENGTH_MEASURE( 1.000000000000000082E-05 ), #1780, 'distance_accuracy_value', 'NONE');
#2837 = PRODUCT_RELATED_PRODUCT_CATEGORY ( 'part', '', ( #1790 ) ) ;
#2838 = PRODUCT_DEFINITION_FORMATION_WITH_SPECIFIED_SOURCE ( 'ANY', '', #235, .NOT_KNOWN. ) ;
#2839 = ITEM_DEFINED_TRANSFORMATION ( 'NONE', 'NONE', #1157,  #3111 ) ;
#2840 = EDGE_LOOP ( 'NONE', ( #297, #1491, #1081, #1094, #335 ) ) ;
#2841 = CYLINDRICAL_SURFACE ( 'NONE', #536, 2.500000000000009326 ) ;
#2842 = UNCERTAINTY_MEASURE_WITH_UNIT (LENGTH_MEASURE( 1.000000000000000082E-05 ), #747, 'distance_accuracy_value', 'NONE');
#2843 =( NAMED_UNIT ( * ) SI_UNIT ( $, .STERADIAN. ) SOLID_ANGLE_UNIT ( ) );
#2844 = ORIENTED_EDGE ( 'NONE', *, *, #32, .T. ) ;
#2845 =( NAMED_UNIT ( * ) PLANE_ANGLE_UNIT ( ) SI_UNIT ( $, .RADIAN. ) );
#2846 = DIRECTION ( 'NONE',  ( 0.000000000000000000, 0.000000000000000000, 1.000000000000000000 ) ) ;
#2847 = DIRECTION ( 'NONE',  ( -0.000000000000000000, -0.000000000000000000, 1.000000000000000000 ) ) ;
#2848 = EDGE_CURVE ( 'NONE', #3236, #1126, #1024, .T. ) ;
#2849 = PLANE ( 'NONE',  #2384 ) ;
#2850 = DIRECTION ( 'NONE',  ( -0.000000000000000000, 1.000000000000000000, -0.000000000000000000 ) ) ;
#2851 = ORIENTED_EDGE ( 'NONE', *, *, #1021, .T. ) ;
#2852 = ORIENTED_EDGE ( 'NONE', *, *, #159, .F. ) ;
#2853 = EDGE_CURVE ( 'NONE', #2252, #595, #979, .T. ) ;
#2854 = FACE_OUTER_BOUND ( 'NONE', #1671, .T. ) ;
#2855 = VERTEX_POINT ( 'NONE', #1809 ) ;
#2856 = PLANE ( 'NONE',  #586 ) ;
#2857 = ORIENTED_EDGE ( 'NONE', *, *, #2314, .F. ) ;
#2858 = DIRECTION ( 'NONE',  ( 1.000000000000000000, 0.000000000000000000, 0.000000000000000000 ) ) ;
#2859 =( NAMED_UNIT ( * ) PLANE_ANGLE_UNIT ( ) SI_UNIT ( $, .RADIAN. ) );
#2860 = DIRECTION ( 'NONE',  ( 1.000000000000000000, 0.000000000000000000, 0.000000000000000000 ) ) ;
#2861 = FACE_OUTER_BOUND ( 'NONE', #3361, .T. ) ;
#2862 = FACE_OUTER_BOUND ( 'NONE', #2871, .T. ) ;
#2863 = EDGE_CURVE ( 'NONE', #617, #2775, #593, .T. ) ;
#2864 = LINE ( 'NONE', #799, #925 ) ;
#2865 = ORIENTED_EDGE ( 'NONE', *, *, #1288, .F. ) ;
#2866 = EDGE_LOOP ( 'NONE', ( #2916, #3354, #1169, #2917 ) ) ;
#2867 = DIRECTION ( 'NONE',  ( 0.000000000000000000, 0.000000000000000000, 1.000000000000000000 ) ) ;
#2868 = EDGE_CURVE ( 'NONE', #2129, #625, #2561, .T. ) ;
#2869 = EDGE_LOOP ( 'NONE', ( #1542, #3037, #2076, #526 ) ) ;
#2870 = CARTESIAN_POINT ( 'NONE',  ( -44.99999999999999289, 52.00000000000000711, 7.850000000000005862 ) ) ;
#2871 = EDGE_LOOP ( 'NONE', ( #888, #2908 ) ) ;
#2872 = VECTOR ( 'NONE', #3310, 1000.000000000000000 ) ;
#2873 = VECTOR ( 'NONE', #1601, 999.9999999999998863 ) ;
#2874 = CARTESIAN_POINT ( 'NONE',  ( -45.00000000000000000, 45.00000000000000711, -11.99999999999999645 ) ) ;
#2875 = AXIS2_PLACEMENT_3D ( 'NONE', #2429, #539, #2381 ) ;
#2876 = EDGE_CURVE ( 'NONE', #2078, #3240, #819, .T. ) ;
#2877 = VECTOR ( 'NONE', #3076, 1000.000000000000000 ) ;
#2878 = DIRECTION ( 'NONE',  ( 0.000000000000000000, 0.000000000000000000, 1.000000000000000000 ) ) ;
#2879 = DIRECTION ( 'NONE',  ( -0.000000000000000000, 1.000000000000000000, -0.000000000000000000 ) ) ;
#2880 = LINE ( 'NONE', #274, #269 ) ;
#2881 = AXIS2_PLACEMENT_3D ( 'NONE', #2708, #1419, #342 ) ;
#2882 = PRODUCT_DEFINITION_SHAPE ( 'NONE', 'NONE',  #3376 ) ;
#2883 = DIRECTION ( 'NONE',  ( 0.000000000000000000, 1.000000000000000000, -1.345283343056720273E-15 ) ) ;
#2884 = VECTOR ( 'NONE', #2612, 1000.000000000000000 ) ;
#2885 = ORIENTED_EDGE ( 'NONE', *, *, #443, .F. ) ;
#2886 = ORIENTED_EDGE ( 'NONE', *, *, #2521, .F. ) ;
#2887 = CARTESIAN_POINT ( 'NONE',  ( 2.000000000000000000, 1.773042676681340524, -2.059984127722458425E-15 ) ) ;
#2888 = AXIS2_PLACEMENT_3D ( 'NONE', #3140, #1075, #1019 ) ;
#2889 =( GEOMETRIC_REPRESENTATION_CONTEXT ( 3 ) GLOBAL_UNCERTAINTY_ASSIGNED_CONTEXT ( ( #1711 ) ) GLOBAL_UNIT_ASSIGNED_CONTEXT ( ( #3067, #2296, #1829 ) ) REPRESENTATION_CONTEXT ( 'NONE', 'WORKASPACE' ) );
#2890 = ORIENTED_EDGE ( 'NONE', *, *, #2827, .F. ) ;
#2891 = EDGE_CURVE ( 'NONE', #2959, #1297, #1283, .T. ) ;
#2892 = DIRECTION ( 'NONE',  ( 0.000000000000000000, 0.4999999999999989453, -0.8660254037844391517 ) ) ;
#2893 = ORIENTED_EDGE ( 'NONE', *, *, #1727, .F. ) ;
#2894 = EDGE_LOOP ( 'NONE', ( #3343, #1057, #1920, #1766 ) ) ;
#2895 = FACE_OUTER_BOUND ( 'NONE', #2697, .T. ) ;
#2896 =( NAMED_UNIT ( * ) SI_UNIT ( $, .STERADIAN. ) SOLID_ANGLE_UNIT ( ) );
#2897 = CARTESIAN_POINT ( 'NONE',  ( -44.99999999999999289, 45.00000000000000711, 10.00000000000000533 ) ) ;
#2898 = CARTESIAN_POINT ( 'NONE',  ( -50.00000000000000000, 120.0000000000000142, 5.000000000000004441 ) ) ;
#2899 = CARTESIAN_POINT ( 'NONE',  ( 4.000000000000003553, 0.000000000000000000, 0.000000000000000000 ) ) ;
#2900 = APPLICATION_CONTEXT ( 'automotive_design' ) ;
#2901 = ORIENTED_EDGE ( 'NONE', *, *, #3125, .F. ) ;
#2902 = EDGE_LOOP ( 'NONE', ( #1824, #1135, #411 ) ) ;
#2903 = DIRECTION ( 'NONE',  ( 0.000000000000000000, -1.000000000000000000, 0.000000000000000000 ) ) ;
#2904 = EDGE_LOOP ( 'NONE', ( #1326, #2206, #41, #292 ) ) ;
#2905 = FACE_OUTER_BOUND ( 'NONE', #3286, .T. ) ;
#2906 = EDGE_CURVE ( 'NONE', #78, #2306, #1839, .T. ) ;
#2907 = DIRECTION ( 'NONE',  ( 0.000000000000000000, 0.000000000000000000, 1.000000000000000000 ) ) ;
#2908 = ORIENTED_EDGE ( 'NONE', *, *, #2132, .T. ) ;
#2909 = PRODUCT_DEFINITION_SHAPE ( 'NONE', 'NONE',  #3385 ) ;
#2910 = CARTESIAN_POINT ( 'NONE',  ( -45.00000000000000000, 45.00000000000000711, -9.999999999999994671 ) ) ;
#2911 = EDGE_CURVE ( 'NONE', #1274, #1395, #1305, .T. ) ;
#2912 = FILL_AREA_STYLE_COLOUR ( '', #1634 ) ;
#2913 = DIRECTION ( 'NONE',  ( -1.000000000000000000, -0.000000000000000000, -0.000000000000000000 ) ) ;
#2914 = LINE ( 'NONE', #866, #2995 ) ;
#2915 = DIRECTION ( 'NONE',  ( 0.000000000000000000, -1.000000000000000000, 0.000000000000000000 ) ) ;
#2916 = ORIENTED_EDGE ( 'NONE', *, *, #3153, .T. ) ;
#2917 = ORIENTED_EDGE ( 'NONE', *, *, #1721, .T. ) ;
#2918 = PLANE ( 'NONE',  #922 ) ;
#2919 = CARTESIAN_POINT ( 'NONE',  ( -45.00000000000000000, 50.00000000000000000, -9.999999999999994671 ) ) ;
#2920 = EDGE_CURVE ( 'NONE', #2775, #331, #2864, .T. ) ;
#2921 = ORIENTED_EDGE ( 'NONE', *, *, #195, .F. ) ;
#2922 = DIRECTION ( 'NONE',  ( 0.000000000000000000, 0.000000000000000000, 1.000000000000000000 ) ) ;
#2923 = CLOSED_SHELL ( 'NONE', ( #2071, #1243, #518, #2458 ) ) ;
#2924 = DIRECTION ( 'NONE',  ( 0.000000000000000000, 0.000000000000000000, 1.000000000000000000 ) ) ;
#2925 = ORIENTED_EDGE ( 'NONE', *, *, #295, .T. ) ;
#2926 = DIRECTION ( 'NONE',  ( 0.000000000000000000, 0.000000000000000000, 1.000000000000000000 ) ) ;
#2927 = DIRECTION ( 'NONE',  ( 1.000000000000000000, 0.000000000000000000, 0.000000000000000000 ) ) ;
#2928 = DIRECTION ( 'NONE',  ( -0.000000000000000000, 1.000000000000000000, -0.000000000000000000 ) ) ;
#2929 = ADVANCED_FACE ( 'NONE', ( #2338 ), #291, .T. ) ;
#2930 = CIRCLE ( 'NONE', #97, 7.500000000000000000 ) ;
#2931 = VECTOR ( 'NONE', #558, 1000.000000000000000 ) ;
#2932 = CARTESIAN_POINT ( 'NONE',  ( 66.99999999999997158, -5.000000000000000000, 39.50000000000000000 ) ) ;
#2933 = ORIENTED_EDGE ( 'NONE', *, *, #2211, .F. ) ;
#2934 = AXIS2_PLACEMENT_3D ( 'NONE', #1399, #2154, #3187 ) ;
#2935 = VECTOR ( 'NONE', #1675, 1000.000000000000000 ) ;
#2936 = EDGE_LOOP ( 'NONE', ( #461, #2941, #26 ) ) ;
#2937 = DIRECTION ( 'NONE',  ( 1.000000000000000000, -0.000000000000000000, 6.938893903907228378E-16 ) ) ;
#2938 = CIRCLE ( 'NONE', #2829, 3.500000000000000000 ) ;
#2939 = VECTOR ( 'NONE', #1620, 999.9999999999998863 ) ;
#2940 = CARTESIAN_POINT ( 'NONE',  ( -75.00000000000000000, 50.00000000000000000, 50.00000000000000000 ) ) ;
#2941 = ORIENTED_EDGE ( 'NONE', *, *, #1667, .T. ) ;
#2942 = LINE ( 'NONE', #1425, #2173 ) ;
#2943 = EDGE_CURVE ( 'NONE', #436, #2252, #2938, .T. ) ;
#2944 = UNCERTAINTY_MEASURE_WITH_UNIT (LENGTH_MEASURE( 1.000000000000000082E-05 ), #447, 'distance_accuracy_value', 'NONE');
#2945 = MANIFOLD_SOLID_BREP ( 'Extrude-Thin1', #2105 ) ;
#2946 = ORIENTED_EDGE ( 'NONE', *, *, #511, .T. ) ;
#2947 = COLOUR_RGB ( '',0.8941176470588234615, 0.8941176470588234615, 0.8941176470588234615 ) ;
#2948 = DIRECTION ( 'NONE',  ( 0.000000000000000000, 0.000000000000000000, 1.000000000000000000 ) ) ;
#2949 = AXIS2_PLACEMENT_3D ( 'NONE', #843, #2924, #434 ) ;
#2950 = CARTESIAN_POINT ( 'NONE',  ( 44.99999999999999289, 50.00000000000000000, -12.00000000000000711 ) ) ;
#2951 = CARTESIAN_POINT ( 'NONE',  ( -44.99999999999999289, 50.00000000000000000, 10.00000000000000533 ) ) ;
#2952 = CARTESIAN_POINT ( 'NONE',  ( -66.99999999999997158, 0.000000000000000000, 44.49999999999999289 ) ) ;
#2953 = ADVANCED_FACE ( 'NONE', ( #623 ), #1333, .F. ) ;
#2954 = EDGE_LOOP ( 'NONE', ( #1133, #1184 ) ) ;
#2955 = ORIENTED_EDGE ( 'NONE', *, *, #2599, .F. ) ;
#2956 = DIRECTION ( 'NONE',  ( 0.000000000000000000, 0.000000000000000000, 1.000000000000000000 ) ) ;
#2957 = CARTESIAN_POINT ( 'NONE',  ( 0.000000000000000000, 52.00000000000000711, 0.000000000000000000 ) ) ;
#2958 = EDGE_CURVE ( 'NONE', #3122, #1345, #1102, .T. ) ;
#2959 = VERTEX_POINT ( 'NONE', #2137 ) ;
#2960 = LINE ( 'NONE', #2425, #2604 ) ;
#2961 = ORIENTED_EDGE ( 'NONE', *, *, #1080, .F. ) ;
#2962 = DIRECTION ( 'NONE',  ( 0.000000000000000000, -1.000000000000000000, 0.000000000000000000 ) ) ;
#2963 = ADVANCED_FACE ( 'NONE', ( #2150 ), #1394, .T. ) ;
#2964 = CARTESIAN_POINT ( 'NONE',  ( -31.74999999999995737, 0.000000000000000000, 0.000000000000000000 ) ) ;
#2965 = DIRECTION ( 'NONE',  ( 0.000000000000000000, -0.4999999999999991118, 0.8660254037844391517 ) ) ;
#2966 = APPLICATION_CONTEXT ( 'automotive_design' ) ;
#2967 = DIRECTION ( 'NONE',  ( -1.000000000000000000, 0.000000000000000000, -0.000000000000000000 ) ) ;
#2968 = VERTEX_POINT ( 'NONE', #3183 ) ;
#2969 = ORIENTED_EDGE ( 'NONE', *, *, #1304, .T. ) ;
#2970 = FACE_OUTER_BOUND ( 'NONE', #1903, .T. ) ;
#2971 = DIRECTION ( 'NONE',  ( 0.000000000000000000, 1.000000000000000000, -1.345283343056720273E-15 ) ) ;
#2972 = VERTEX_POINT ( 'NONE', #2187 ) ;
#2973 = CARTESIAN_POINT ( 'NONE',  ( -49.99999999999998579, 52.00000000000000711, 15.00000000000000888 ) ) ;
#2974 = ADVANCED_FACE ( 'NONE', ( #3249, #353 ), #1380, .F. ) ;
#2975 = DIRECTION ( 'NONE',  ( 6.123233995736766036E-17, -1.000000000000000000, 0.000000000000000000 ) ) ;
#2976 = VERTEX_POINT ( 'NONE', #323 ) ;
#2977 = CARTESIAN_POINT ( 'NONE',  ( 2.000000000000000000, -0.8865213383406694847, 1.535500000000001419 ) ) ;
#2978 = DIRECTION ( 'NONE',  ( 0.000000000000000000, 0.000000000000000000, -1.000000000000000000 ) ) ;
#2979 = DIRECTION ( 'NONE',  ( 1.000000000000000000, -0.000000000000000000, 6.938893903907229364E-16 ) ) ;
#2980 = PRODUCT_DEFINITION ( 'UNKNOWN', '', #2838, #2466 ) ;
#2981 = CIRCLE ( 'NONE', #474, 1.535500000000000087 ) ;
#2982 = DIRECTION ( 'NONE',  ( 6.938893903907229364E-16, 0.000000000000000000, -1.000000000000000000 ) ) ;
#2983 = CARTESIAN_POINT ( 'NONE',  ( -66.99999999999997158, -5.000000000000000000, -41.99999999999999289 ) ) ;
#2984 = CIRCLE ( 'NONE', #1257, 2.000000000000001776 ) ;
#2985 = FACE_OUTER_BOUND ( 'NONE', #2840, .T. ) ;
#2986 = AXIS2_PLACEMENT_3D ( 'NONE', #441, #2184, #116 ) ;
#2987 = CARTESIAN_POINT ( 'NONE',  ( 2.000000000000000000, 1.773042676681340524, -2.059984127722458425E-15 ) ) ;
#2988 = CIRCLE ( 'NONE', #150, 4.500000000000010658 ) ;
#2989 = AXIS2_PLACEMENT_3D ( 'NONE', #790, #280, #3170 ) ;
#2990 = ORIENTED_EDGE ( 'NONE', *, *, #619, .T. ) ;
#2991 = DIRECTION ( 'NONE',  ( 0.000000000000000000, -1.000000000000000000, 0.000000000000000000 ) ) ;
#2992 = AXIS2_PLACEMENT_3D ( 'NONE', #731, #1536, #1772 ) ;
#2993 = APPLICATION_PROTOCOL_DEFINITION ( 'draft international standard', 'automotive_design', 1998, #1857 ) ;
#2994 = VECTOR ( 'NONE', #786, 1000.000000000000000 ) ;
#2995 = VECTOR ( 'NONE', #68, 1000.000000000000000 ) ;
#2996 = ORIENTED_EDGE ( 'NONE', *, *, #1411, .T. ) ;
#2997 = EDGE_CURVE ( 'NONE', #774, #2320, #1119, .T. ) ;
#2998 = CARTESIAN_POINT ( 'NONE',  ( 66.99999999999997158, -5.000000000000000000, -41.99999999999999289 ) ) ;
#2999 = COLOUR_RGB ( '',0.8941176470588234615, 0.8941176470588234615, 0.8941176470588234615 ) ;
#3000 =( LENGTH_UNIT ( ) NAMED_UNIT ( * ) SI_UNIT ( .MILLI., .METRE. ) );
#3001 = COLOUR_RGB ( '',1.000000000000000000, 0.9490196078431372140, 0.9098039215686274384 ) ;
#3002 = DIRECTION ( 'NONE',  ( -1.000000000000000000, -0.000000000000000000, -0.000000000000000000 ) ) ;
#3003 = CARTESIAN_POINT ( 'NONE',  ( 4.200000000000001954, 2.694222958124178486E-16, 2.200000000000001066 ) ) ;
#3004 = ITEM_DEFINED_TRANSFORMATION ( 'NONE', 'NONE', #1641,  #3111 ) ;
#3005 = FACE_OUTER_BOUND ( 'NONE', #2904, .T. ) ;
#3006 = DIRECTION ( 'NONE',  ( 0.000000000000000000, 0.000000000000000000, 1.000000000000000000 ) ) ;
#3007 = CARTESIAN_POINT ( 'NONE',  ( -45.00000000000000000, 52.00000000000000711, -9.999999999999994671 ) ) ;
#3008 = ORIENTED_EDGE ( 'NONE', *, *, #2806, .F. ) ;
#3009 = DIRECTION ( 'NONE',  ( 0.000000000000000000, 0.000000000000000000, 1.000000000000000000 ) ) ;
#3010 = APPLICATION_PROTOCOL_DEFINITION ( 'draft international standard', 'automotive_design', 1998, #2900 ) ;
#3011 = ORIENTED_EDGE ( 'NONE', *, *, #2243, .F. ) ;
#3012 = DIRECTION ( 'NONE',  ( -0.000000000000000000, 1.000000000000000000, -0.000000000000000000 ) ) ;
#3013 = EDGE_CURVE ( 'NONE', #1395, #1274, #378, .T. ) ;
#3014 =( NAMED_UNIT ( * ) SI_UNIT ( $, .STERADIAN. ) SOLID_ANGLE_UNIT ( ) );
#3015 = FACE_BOUND ( 'NONE', #258, .T. ) ;
#3016 = CARTESIAN_POINT ( 'NONE',  ( -45.00000000000000000, 50.00000000000000000, -7.999999999999992895 ) ) ;
#3017 = EDGE_CURVE ( 'NONE', #1926, #2054, #2703, .T. ) ;
#3018 = DIRECTION ( 'NONE',  ( 0.000000000000000000, 0.000000000000000000, 1.000000000000000000 ) ) ;
#3019 = CARTESIAN_POINT ( 'NONE',  ( 9.610000000000013642, 0.000000000000000000, 2.000000000000000888 ) ) ;
#3020 = FACE_OUTER_BOUND ( 'NONE', #355, .T. ) ;
#3021 = SURFACE_STYLE_USAGE ( .BOTH. , #2797 ) ;
#3022 = ORIENTED_EDGE ( 'NONE', *, *, #220, .F. ) ;
#3023 = FACE_OUTER_BOUND ( 'NONE', #726, .T. ) ;
#3024 = EDGE_CURVE ( 'NONE', #1965, #28, #2179, .T. ) ;
#3025 = APPLICATION_PROTOCOL_DEFINITION ( 'draft international standard', 'automotive_design', 1998, #1167 ) ;
#3026 = VERTEX_POINT ( 'NONE', #2932 ) ;
#3027 = CARTESIAN_POINT ( 'NONE',  ( 2.000000000000000000, 0.8865213383406715941, 1.535499999999999199 ) ) ;
#3028 = EDGE_LOOP ( 'NONE', ( #2070, #2857, #908, #512, #2043 ) ) ;
#3029 = CARTESIAN_POINT ( 'NONE',  ( 4.000000000000000000, 3.500000000000000000, 0.000000000000000000 ) ) ;
#3030 = CARTESIAN_POINT ( 'NONE',  ( -50.00000000000000000, 52.00000000000000711, 5.000000000000004441 ) ) ;
#3031 = DIRECTION ( 'NONE',  ( 0.000000000000000000, -1.000000000000000000, 0.000000000000000000 ) ) ;
#3032 = DIRECTION ( 'NONE',  ( -1.000000000000000000, -0.000000000000000000, -0.000000000000000000 ) ) ;
#3033 = EDGE_CURVE ( 'NONE', #1965, #2968, #1888, .T. ) ;
#3034 = DIRECTION ( 'NONE',  ( -0.000000000000000000, 1.000000000000000000, -0.000000000000000000 ) ) ;
#3035 = DIRECTION ( 'NONE',  ( 0.000000000000000000, -1.000000000000000000, 0.000000000000000000 ) ) ;
#3036 = CIRCLE ( 'NONE', #913, 2.000000000000001776 ) ;
#3037 = ORIENTED_EDGE ( 'NONE', *, *, #2529, .T. ) ;
#3038 = CARTESIAN_POINT ( 'NONE',  ( 66.99999999999997158, -5.000000000000000000, 41.99999999999999289 ) ) ;
#3039 = CONICAL_SURFACE ( 'NONE', #1515, 2.000000000000001776, 1.029744258676657642 ) ;
#3040 = CIRCLE ( 'NONE', #973, 6.812556682370379590 ) ;
#3041 = DIRECTION ( 'NONE',  ( 0.000000000000000000, 0.000000000000000000, -1.000000000000000000 ) ) ;
#3042 = ORIENTED_EDGE ( 'NONE', *, *, #1311, .T. ) ;
#3043 = AXIS2_PLACEMENT_3D ( 'NONE', #2620, #282, #2396 ) ;
#3044 = PRODUCT_RELATED_PRODUCT_CATEGORY ( 'part', '', ( #1577 ) ) ;
#3045 = AXIS2_PLACEMENT_3D ( 'NONE', #1976, #3034, #3251 ) ;
#3046 = DIRECTION ( 'NONE',  ( 0.000000000000000000, 0.000000000000000000, -1.000000000000000000 ) ) ;
#3047 = VECTOR ( 'NONE', #371, 1000.000000000000000 ) ;
#3048 = AXIS2_PLACEMENT_3D ( 'NONE', #473, #2831, #1007 ) ;
#3049 = FILL_AREA_STYLE ('',( #2721 ) ) ;
#3050 = ORIENTED_EDGE ( 'NONE', *, *, #3033, .F. ) ;
#3051 = FACE_OUTER_BOUND ( 'NONE', #2644, .T. ) ;
#3052 = DIRECTION ( 'NONE',  ( 0.000000000000000000, -1.000000000000000000, 0.000000000000000000 ) ) ;
#3053 = SURFACE_STYLE_USAGE ( .BOTH. , #1719 ) ;
#3054 =( GEOMETRIC_REPRESENTATION_CONTEXT ( 3 ) GLOBAL_UNCERTAINTY_ASSIGNED_CONTEXT ( ( #725 ) ) GLOBAL_UNIT_ASSIGNED_CONTEXT ( ( #364, #2454, #2896 ) ) REPRESENTATION_CONTEXT ( 'NONE', 'WORKASPACE' ) );
#3055 = DIRECTION ( 'NONE',  ( 0.000000000000000000, 0.000000000000000000, -1.000000000000000000 ) ) ;
#3056 = LINE ( 'NONE', #2215, #1793 ) ;
#3057 = AXIS2_PLACEMENT_3D ( 'NONE', #654, #1698, #1677 ) ;
#3058 = EDGE_CURVE ( 'NONE', #2460, #2106, #1925, .T. ) ;
#3059 = CARTESIAN_POINT ( 'NONE',  ( -54.99999999999995026, 130.0000000000000000, 5.000000000000004441 ) ) ;
#3060 = ORIENTED_EDGE ( 'NONE', *, *, #691, .F. ) ;
#3061 = ORIENTED_EDGE ( 'NONE', *, *, #1651, .F. ) ;
#3062 = DIRECTION ( 'NONE',  ( -6.938893903907228378E-16, 0.000000000000000000, 1.000000000000000000 ) ) ;
#3063 = EDGE_CURVE ( 'NONE', #2394, #684, #2418, .T. ) ;
#3064 = ITEM_DEFINED_TRANSFORMATION ( 'NONE', 'NONE', #822,  #3111 ) ;
#3065 = ORIENTED_EDGE ( 'NONE', *, *, #1950, .T. ) ;
#3066 = CARTESIAN_POINT ( 'NONE',  ( 0.000000000000000000, 50.00000000000000000, 0.000000000000000000 ) ) ;
#3067 =( LENGTH_UNIT ( ) NAMED_UNIT ( * ) SI_UNIT ( .MILLI., .METRE. ) );
#3068 = ORIENTED_EDGE ( 'NONE', *, *, #1182, .T. ) ;
#3069 =( LENGTH_UNIT ( ) NAMED_UNIT ( * ) SI_UNIT ( .MILLI., .METRE. ) );
#3070 = EDGE_CURVE ( 'NONE', #3133, #3137, #305, .T. ) ;
#3071 = CARTESIAN_POINT ( 'NONE',  ( 2.000000000000000000, 1.773042676681340524, -2.059984127722458425E-15 ) ) ;
#3072 = DIRECTION ( 'NONE',  ( -0.000000000000000000, 1.000000000000000000, -0.000000000000000000 ) ) ;
#3073 = DIRECTION ( 'NONE',  ( 1.000000000000000000, 0.000000000000000000, 0.000000000000000000 ) ) ;
#3074 = EDGE_LOOP ( 'NONE', ( #2388, #3235 ) ) ;
#3075 = ORIENTED_EDGE ( 'NONE', *, *, #708, .F. ) ;
#3076 = DIRECTION ( 'NONE',  ( 0.000000000000000000, -1.000000000000000000, 9.783878858594328898E-16 ) ) ;
#3077 = PRODUCT_DEFINITION_CONTEXT ( 'detailed design', #2900, 'design' ) ;
#3078 = VERTEX_POINT ( 'NONE', #2952 ) ;
#3079 = EDGE_CURVE ( 'NONE', #1554, #1605, #1201, .T. ) ;
#3080 = CARTESIAN_POINT ( 'NONE',  ( -66.99999999999997158, -5.000000000000000000, 41.99999999999999289 ) ) ;
#3081 = PRESENTATION_STYLE_ASSIGNMENT (( #762 ) ) ;
#3082 = ORIENTED_EDGE ( 'NONE', *, *, #2784, .F. ) ;
#3083 = DIRECTION ( 'NONE',  ( -0.5000000000000061062, 1.060575238724902601E-16, -0.8660254037844351549 ) ) ;
#3084 = DIRECTION ( 'NONE',  ( -0.000000000000000000, -1.000000000000000000, -0.000000000000000000 ) ) ;
#3085 = CARTESIAN_POINT ( 'NONE',  ( 9.610000000000013642, 0.000000000000000000, 0.000000000000000000 ) ) ;
#3086 = FACE_OUTER_BOUND ( 'NONE', #3188, .T. ) ;
#3087 = VECTOR ( 'NONE', #394, 1000.000000000000000 ) ;
#3088 = DIRECTION ( 'NONE',  ( 0.000000000000000000, 0.000000000000000000, -1.000000000000000000 ) ) ;
#3089 = ORIENTED_EDGE ( 'NONE', *, *, #2853, .T. ) ;
#3090 = EDGE_LOOP ( 'NONE', ( #3243, #1290 ) ) ;
#3091 = FACE_OUTER_BOUND ( 'NONE', #732, .T. ) ;
#3092 = AXIS2_PLACEMENT_3D ( 'NONE', #3350, #197, #1020 ) ;
#3093 = ITEM_DEFINED_TRANSFORMATION ( 'NONE', 'NONE', #169,  #3111 ) ;
#3094 = ORIENTED_EDGE ( 'NONE', *, *, #2958, .T. ) ;
#3095 = VECTOR ( 'NONE', #2587, 1000.000000000000000 ) ;
#3096 = LINE ( 'NONE', #706, #643 ) ;
#3097 = VECTOR ( 'NONE', #1017, 1000.000000000000000 ) ;
#3098 = ADVANCED_FACE ( 'NONE', ( #2404 ), #2386, .F. ) ;
#3099 = FILL_AREA_STYLE ('',( #1309 ) ) ;
#3100 = VECTOR ( 'NONE', #2672, 1000.000000000000000 ) ;
#3101 = AXIS2_PLACEMENT_3D ( 'NONE', #1660, #1185, #1980 ) ;
#3102 = EDGE_LOOP ( 'NONE', ( #2409, #947, #2925, #2319, #2509 ) ) ;
#3103 = PRODUCT_DEFINITION_SHAPE ( 'NONE', 'NONE',  #2980 ) ;
#3104 = CARTESIAN_POINT ( 'NONE',  ( -44.99999999999999289, 52.00000000000000711, 10.00000000000000533 ) ) ;
#3105 = AXIS2_PLACEMENT_3D ( 'NONE', #1827, #1352, #1173 ) ;
#3106 = AXIS2_PLACEMENT_3D ( 'NONE', #1296, #2032, #1836 ) ;
#3107 = DIRECTION ( 'NONE',  ( 0.000000000000000000, 0.000000000000000000, 1.000000000000000000 ) ) ;
#3108 = MECHANICAL_DESIGN_GEOMETRIC_PRESENTATION_REPRESENTATION (  '', ( #2009 ), #1632 ) ;
#3109 = CARTESIAN_POINT ( 'NONE',  ( -39.00000000000000000, 52.00000000000000711, 5.000000000000004441 ) ) ;
#3110 = DIRECTION ( 'NONE',  ( 0.000000000000000000, -1.000000000000000000, 0.000000000000000000 ) ) ;
#3111 = AXIS2_PLACEMENT_3D ( 'NONE', #1871, #3207, #2639 ) ;
#3112 = DIRECTION ( 'NONE',  ( 0.000000000000000000, 0.000000000000000000, 1.000000000000000000 ) ) ;
#3113 = ORIENTED_EDGE ( 'NONE', *, *, #3182, .T. ) ;
#3114 = ORIENTED_EDGE ( 'NONE', *, *, #181, .F. ) ;
#3115 = DIRECTION ( 'NONE',  ( -0.7071067811865355823, 8.659560562355079537E-17, -0.7071067811865595631 ) ) ;
#3116 =( GEOMETRIC_REPRESENTATION_CONTEXT ( 3 ) GLOBAL_UNCERTAINTY_ASSIGNED_CONTEXT ( ( #2565 ) ) GLOBAL_UNIT_ASSIGNED_CONTEXT ( ( #567, #1388, #1091 ) ) REPRESENTATION_CONTEXT ( 'NONE', 'WORKASPACE' ) );
#3117 = CONTEXT_DEPENDENT_SHAPE_REPRESENTATION ( #1073, #2337 ) ;
#3118 = EDGE_LOOP ( 'NONE', ( #386, #2921, #254, #2057 ) ) ;
#3119 = CARTESIAN_POINT ( 'NONE',  ( -39.00000000000000000, 117.0000000000000000, -5.999999999999995559 ) ) ;
#3120 = UNCERTAINTY_MEASURE_WITH_UNIT (LENGTH_MEASURE( 1.000000000000000082E-05 ), #897, 'distance_accuracy_value', 'NONE');
#3121 = PRESENTATION_STYLE_ASSIGNMENT (( #2326 ) ) ;
#3122 = VERTEX_POINT ( 'NONE', #53 ) ;
#3123 = CARTESIAN_POINT ( 'NONE',  ( -50.00000000000000000, 50.00000000000000000, 5.000000000000004441 ) ) ;
#3124 =( NAMED_UNIT ( * ) SI_UNIT ( $, .STERADIAN. ) SOLID_ANGLE_UNIT ( ) );
#3125 = EDGE_CURVE ( 'NONE', #84, #1345, #339, .T. ) ;
#3126 = CARTESIAN_POINT ( 'NONE',  ( -66.99999999999997158, 0.000000000000000000, 39.49999999999998579 ) ) ;
#3127 = CARTESIAN_POINT ( 'NONE',  ( 44.99999999999999289, 45.00000000000000711, -10.00000000000000533 ) ) ;
#3128 = FACE_OUTER_BOUND ( 'NONE', #64, .T. ) ;
#3129 = EDGE_CURVE ( 'NONE', #2643, #2174, #3214, .T. ) ;
#3130 = ORIENTED_EDGE ( 'NONE', *, *, #3273, .T. ) ;
#3131 = ORIENTED_EDGE ( 'NONE', *, *, #3134, .F. ) ;
#3132 = FACE_OUTER_BOUND ( 'NONE', #3359, .T. ) ;
#3133 = VERTEX_POINT ( 'NONE', #713 ) ;
#3134 = EDGE_CURVE ( 'NONE', #594, #2691, #1151, .T. ) ;
#3135 = DIRECTION ( 'NONE',  ( -0.000000000000000000, 1.000000000000000000, -0.000000000000000000 ) ) ;
#3136 =( NAMED_UNIT ( * ) SI_UNIT ( $, .STERADIAN. ) SOLID_ANGLE_UNIT ( ) );
#3137 = VERTEX_POINT ( 'NONE', #2247 ) ;
#3138 = CARTESIAN_POINT ( 'NONE',  ( 2.000000000000000000, 0.000000000000000000, 0.000000000000000000 ) ) ;
#3139 = CARTESIAN_POINT ( 'NONE',  ( 10.00000000000000178, 2.210487472460973191E-16, -1.610000000000000098 ) ) ;
#3140 = CARTESIAN_POINT ( 'NONE',  ( 2.000000000000000000, 0.000000000000000000, 0.000000000000000000 ) ) ;
#3141 = CARTESIAN_POINT ( 'NONE',  ( 44.99999999999999289, 50.00000000000000000, -10.00000000000000533 ) ) ;
#3142 = DIRECTION ( 'NONE',  ( 0.000000000000000000, 0.000000000000000000, -1.000000000000000000 ) ) ;
#3143 = CARTESIAN_POINT ( 'NONE',  ( 0.000000000000000000, -0.8865213383406694847, 1.535500000000001419 ) ) ;
#3144 = EDGE_CURVE ( 'NONE', #309, #3122, #2486, .T. ) ;
#3145 = EDGE_LOOP ( 'NONE', ( #1138, #778, #1224, #340 ) ) ;
#3146 = ORIENTED_EDGE ( 'NONE', *, *, #674, .F. ) ;
#3147 = DIRECTION ( 'NONE',  ( 0.000000000000000000, -1.000000000000000000, 0.000000000000000000 ) ) ;
#3148 = CLOSED_SHELL ( 'NONE', ( #2157, #1040, #2671, #918, #528, #846, #5, #570, #556, #2698, #389, #1860, #1107, #1473, #2679, #1358, #2489, #1346, #2511, #2308, #1422, #1127, #588, #1638, #3276, #187, #804 ) ) ;
#3149 = ADVANCED_BREP_SHAPE_REPRESENTATION ( '', ( #573, #3111 ), #1101 ) ;
#3150 = EDGE_LOOP ( 'NONE', ( #57, #2424, #440 ) ) ;
#3151 = FACE_OUTER_BOUND ( 'NONE', #1883, .T. ) ;
#3152 = CARTESIAN_POINT ( 'NONE',  ( 0.000000000000000000, 0.000000000000000000, 0.000000000000000000 ) ) ;
#3153 = EDGE_CURVE ( 'NONE', #2464, #902, #2473, .T. ) ;
#3154 = VERTEX_POINT ( 'NONE', #1755 ) ;
#3155 = AXIS2_PLACEMENT_3D ( 'NONE', #2313, #1546, #1042 ) ;
#3156 = DIRECTION ( 'NONE',  ( 0.000000000000000000, -1.000000000000000000, 0.000000000000000000 ) ) ;
#3157 = AXIS2_PLACEMENT_3D ( 'NONE', #2413, #300, #2637 ) ;
#3158 = AXIS2_PLACEMENT_3D ( 'NONE', #1593, #527, #2867 ) ;
#3159 = DIRECTION ( 'NONE',  ( 1.000000000000000000, 0.000000000000000000, 0.000000000000000000 ) ) ;
#3160 = DIRECTION ( 'NONE',  ( -1.000000000000000000, -0.000000000000000000, -0.000000000000000000 ) ) ;
#3161 = AXIS2_PLACEMENT_3D ( 'NONE', #1485, #1251, #172 ) ;
#3162 = DIRECTION ( 'NONE',  ( 0.000000000000000000, 0.000000000000000000, 1.000000000000000000 ) ) ;
#3163 = AXIS2_PLACEMENT_3D ( 'NONE', #2098, #1046, #2335 ) ;
#3164 = PRODUCT_DEFINITION_SHAPE ( 'NONE', 'NONE',  #3386 ) ;
#3165 = SHAPE_REPRESENTATION ( 'MAS-192', ( #1476, #2347, #1105, #114, #2621, #497, #710, #2949, #822, #549, #2726, #1157, #1641, #2566, #169, #3057 ), #1802 ) ;
#3166 = PRESENTATION_STYLE_ASSIGNMENT (( #1791 ) ) ;
#3167 = VECTOR ( 'NONE', #1215, 1000.000000000000000 ) ;
#3168 = EDGE_LOOP ( 'NONE', ( #844, #1366, #1655, #2181 ) ) ;
#3169 = ORIENTED_EDGE ( 'NONE', *, *, #1869, .F. ) ;
#3170 = DIRECTION ( 'NONE',  ( -1.000000000000000000, 0.000000000000000000, -0.000000000000000000 ) ) ;
#3171 = MANIFOLD_SOLID_BREP ( 'Boss-Extrude1', #2923 ) ;
#3172 = AXIS2_PLACEMENT_3D ( 'NONE', #69, #2165, #574 ) ;
#3173 = ADVANCED_FACE ( 'NONE', ( #3263 ), #1690, .F. ) ;
#3174 = VERTEX_POINT ( 'NONE', #642 ) ;
#3175 = DIRECTION ( 'NONE',  ( -0.000000000000000000, 1.000000000000000000, -0.000000000000000000 ) ) ;
#3176 = ADVANCED_FACE ( 'NONE', ( #1196 ), #662, .T. ) ;
#3177 = ORIENTED_EDGE ( 'NONE', *, *, #2595, .F. ) ;
#3178 = DIRECTION ( 'NONE',  ( -1.000000000000000000, -0.000000000000000000, -0.000000000000000000 ) ) ;
#3179 = FILL_AREA_STYLE ('',( #2912 ) ) ;
#3180 = CARTESIAN_POINT ( 'NONE',  ( -49.99999999999999289, 52.00000000000000711, 5.000000000000007994 ) ) ;
#3181 = DIRECTION ( 'NONE',  ( 1.000000000000000000, 0.000000000000000000, 0.000000000000000000 ) ) ;
#3182 = EDGE_CURVE ( 'NONE', #1968, #1875, #2727, .T. ) ;
#3183 = CARTESIAN_POINT ( 'NONE',  ( 4.200000000000001954, 2.449293598294707893E-16, -2.000000000000000888 ) ) ;
#3184 = ORIENTED_EDGE ( 'NONE', *, *, #343, .F. ) ;
#3185 = EDGE_LOOP ( 'NONE', ( #1594, #1478, #192, #381 ) ) ;
#3186 = PLANE ( 'NONE',  #1148 ) ;
#3187 = DIRECTION ( 'NONE',  ( 0.000000000000000000, 0.000000000000000000, 1.000000000000000000 ) ) ;
#3188 = EDGE_LOOP ( 'NONE', ( #1048, #1679, #3347, #839 ) ) ;
#3189 = LINE ( 'NONE', #2127, #921 ) ;
#3190 = VERTEX_POINT ( 'NONE', #690 ) ;
#3191 = ADVANCED_FACE ( 'NONE', ( #393 ), #1974, .T. ) ;
#3192 = DIRECTION ( 'NONE',  ( 0.000000000000000000, -0.5000000000000011102, -0.8660254037844379305 ) ) ;
#3193 = CARTESIAN_POINT ( 'NONE',  ( 0.1999999999999987899, 0.000000000000000000, 0.000000000000000000 ) ) ;
#3194 = DIRECTION ( 'NONE',  ( -0.000000000000000000, -1.000000000000000000, -0.000000000000000000 ) ) ;
#3195 = CARTESIAN_POINT ( 'NONE',  ( -51.00000000000000000, 52.00000000000000711, -4.999999999999996447 ) ) ;
#3196 = VERTEX_POINT ( 'NONE', #675 ) ;
#3197 = PRODUCT_DEFINITION ( 'UNKNOWN', '', #1587, #1207 ) ;
#3198 = ORIENTED_EDGE ( 'NONE', *, *, #630, .F. ) ;
#3199 = PLANE ( 'NONE',  #1145 ) ;
#3200 = PLANE ( 'NONE',  #2500 ) ;
#3201 = EDGE_LOOP ( 'NONE', ( #655, #2946 ) ) ;
#3202 = CARTESIAN_POINT ( 'NONE',  ( 10.00000000000000178, 0.000000000000000000, 1.610000000000000098 ) ) ;
#3203 = VERTEX_POINT ( 'NONE', #2754 ) ;
#3204 = FACE_OUTER_BOUND ( 'NONE', #2704, .T. ) ;
#3205 = CIRCLE ( 'NONE', #1512, 1.535500000000000087 ) ;
#3206 = EDGE_CURVE ( 'NONE', #895, #499, #2282, .T. ) ;
#3207 = DIRECTION ( 'NONE',  ( 0.000000000000000000, 0.000000000000000000, 1.000000000000000000 ) ) ;
#3208 = CONICAL_SURFACE ( 'NONE', #965, 2.000000000000001776, 1.029744258676657642 ) ;
#3209 = CARTESIAN_POINT ( 'NONE',  ( -44.99999999999999289, 45.00000000000000711, 12.00000000000000711 ) ) ;
#3210 = CARTESIAN_POINT ( 'NONE',  ( 66.99999999999997158, -5.000000000000000000, 41.99999999999999289 ) ) ;
#3211=STYLED_ITEM('',(#3415),#2021);
#3212 = VECTOR ( 'NONE', #1835, 1000.000000000000000 ) ;
#3213 = EDGE_CURVE ( 'NONE', #3026, #121, #954, .T. ) ;
#3214 = LINE ( 'NONE', #869, #59 ) ;
#3215 = VERTEX_POINT ( 'NONE', #1482 ) ;
#3216 = CONICAL_SURFACE ( 'NONE', #2176, 2.000000000000001776, 1.029744258676657642 ) ;
#3217 = TOROIDAL_SURFACE ( 'NONE', #2823, 2.200000000000001066, 0.2000000000000000111 ) ;
#3218 = ORIENTED_EDGE ( 'NONE', *, *, #1644, .F. ) ;
#3219 = CARTESIAN_POINT ( 'NONE',  ( 66.99999999999997158, -5.000000000000000000, 44.49999999999999289 ) ) ;
#3220 = VECTOR ( 'NONE', #3234, 1000.000000000000000 ) ;
#3221 = VECTOR ( 'NONE', #3266, 1000.000000000000000 ) ;
#3222 = DIRECTION ( 'NONE',  ( -0.000000000000000000, 1.000000000000000000, -0.000000000000000000 ) ) ;
#3223 = ORIENTED_EDGE ( 'NONE', *, *, #1390, .T. ) ;
#3224 = PRESENTATION_LAYER_ASSIGNMENT (  '', '', ( #1259 ) ) ;
#3225 = DIRECTION ( 'NONE',  ( -1.000000000000000000, -0.000000000000000000, -0.000000000000000000 ) ) ;
#3226 = EDGE_CURVE ( 'NONE', #1054, #872, #184, .T. ) ;
#3227 = DIRECTION ( 'NONE',  ( 0.000000000000000000, 0.000000000000000000, 1.000000000000000000 ) ) ;
#3228 = ORIENTED_EDGE ( 'NONE', *, *, #106, .F. ) ;
#3229 = PRODUCT_DEFINITION_FORMATION_WITH_SPECIFIED_SOURCE ( 'ANY', '', #25, .NOT_KNOWN. ) ;
#3230 = DIRECTION ( 'NONE',  ( 0.000000000000000000, 0.000000000000000000, 1.000000000000000000 ) ) ;
#3231 = SURFACE_SIDE_STYLE ('',( #349 ) ) ;
#3232 = LINE ( 'NONE', #899, #1568 ) ;
#3233 = CARTESIAN_POINT ( 'NONE',  ( -44.99999999999999289, 45.00000000000000711, 10.00000000000000533 ) ) ;
#3234 = DIRECTION ( 'NONE',  ( -1.000000000000000000, -0.000000000000000000, -0.000000000000000000 ) ) ;
#3235 = ORIENTED_EDGE ( 'NONE', *, *, #36, .T. ) ;
#3236 = VERTEX_POINT ( 'NONE', #3312 ) ;
#3237 = EDGE_CURVE ( 'NONE', #2972, #594, #968, .T. ) ;
#3238 = CARTESIAN_POINT ( 'NONE',  ( -44.99999999999999289, 50.00000000000000000, 10.00000000000000533 ) ) ;
#3239 = CARTESIAN_POINT ( 'NONE',  ( 4.200000000000001954, 0.000000000000000000, 0.000000000000000000 ) ) ;
#3240 = VERTEX_POINT ( 'NONE', #249 ) ;
#3241 = CARTESIAN_POINT ( 'NONE',  ( -75.00000000000000000, 0.000000000000000000, 50.00000000000000000 ) ) ;
#3242 = PRODUCT_CONTEXT ( 'NONE', #738, 'mechanical' ) ;
#3243 = ORIENTED_EDGE ( 'NONE', *, *, #2186, .F. ) ;
#3244 = ADVANCED_FACE ( 'NONE', ( #289 ), #541, .T. ) ;
#3245 = DIRECTION ( 'NONE',  ( 0.000000000000000000, -1.000000000000000000, 0.000000000000000000 ) ) ;
#3246 = SURFACE_STYLE_USAGE ( .BOTH. , #707 ) ;
#3247 = FACE_OUTER_BOUND ( 'NONE', #1726, .T. ) ;
#3248 = LINE ( 'NONE', #1193, #2872 ) ;
#3249 = FACE_BOUND ( 'NONE', #2188, .T. ) ;
#3250 = ORIENTED_EDGE ( 'NONE', *, *, #698, .F. ) ;
#3251 = DIRECTION ( 'NONE',  ( 0.000000000000000000, 0.000000000000000000, 1.000000000000000000 ) ) ;
#3252 = EDGE_CURVE ( 'NONE', #78, #902, #1769, .T. ) ;
#3253 = FACE_BOUND ( 'NONE', #1389, .T. ) ;
#3254 = ORIENTED_EDGE ( 'NONE', *, *, #2132, .F. ) ;
#3255 = CARTESIAN_POINT ( 'NONE',  ( -66.99999999999997158, 0.000000000000000000, 41.99999999999999289 ) ) ;
#3256 = DIRECTION ( 'NONE',  ( 6.123233995736766036E-17, -1.000000000000000000, 0.000000000000000000 ) ) ;
#3257 =( REPRESENTATION_RELATIONSHIP ('NONE','NONE', #3165, #685 ) REPRESENTATION_RELATIONSHIP_WITH_TRANSFORMATION ( #501 )SHAPE_REPRESENTATION_RELATIONSHIP( ) );
#3258 = EDGE_LOOP ( 'NONE', ( #2380, #372, #1911, #180 ) ) ;
#3259 = CARTESIAN_POINT ( 'NONE',  ( -50.00000000000000000, 120.0000000000000142, 5.000000000000004441 ) ) ;
#3260 = PLANE ( 'NONE',  #1404 ) ;
#3261 = DIRECTION ( 'NONE',  ( 0.000000000000000000, 0.000000000000000000, 1.000000000000000000 ) ) ;
#3262 = CIRCLE ( 'NONE', #2328, 2.000000000000000888 ) ;
#3263 = FACE_OUTER_BOUND ( 'NONE', #1934, .T. ) ;
#3264 = EDGE_LOOP ( 'NONE', ( #2159, #2634, #6, #2349 ) ) ;
#3265 = CIRCLE ( 'NONE', #104, 0.2000000000000000944 ) ;
#3266 = DIRECTION ( 'NONE',  ( -1.000000000000000000, -0.000000000000000000, -0.000000000000000000 ) ) ;
#3267 = VECTOR ( 'NONE', #2978, 1000.000000000000000 ) ;
#3268 = FILL_AREA_STYLE_COLOUR ( '', #1096 ) ;
#3269 = AXIS2_PLACEMENT_3D ( 'NONE', #65, #1599, #2926 ) ;
#3270 = AXIS2_PLACEMENT_3D ( 'NONE', #1066, #3147, #481 ) ;
#3271 = ORIENTED_EDGE ( 'NONE', *, *, #1182, .F. ) ;
#3272 = DIRECTION ( 'NONE',  ( -1.000000000000000000, 0.000000000000000000, 0.000000000000000000 ) ) ;
#3273 = EDGE_CURVE ( 'NONE', #2365, #223, #1958, .T. ) ;
#3274=STYLED_ITEM('',(#3415),#2792);
#3275 = ORIENTED_EDGE ( 'NONE', *, *, #2015, .T. ) ;
#3276 = ADVANCED_FACE ( 'NONE', ( #2626 ), #1548, .F. ) ;
#3277 = FACE_OUTER_BOUND ( 'NONE', #2866, .T. ) ;
#3278 = AXIS2_PLACEMENT_3D ( 'NONE', #3364, #2354, #744 ) ;
#3279 = DIRECTION ( 'NONE',  ( 0.000000000000000000, 0.000000000000000000, -1.000000000000000000 ) ) ;
#3280 = DIRECTION ( 'NONE',  ( -1.000000000000000000, 0.000000000000000000, 0.000000000000000000 ) ) ;
#3281 = DIRECTION ( 'NONE',  ( -0.000000000000000000, -1.000000000000000000, -0.000000000000000000 ) ) ;
#3282 = CYLINDRICAL_SURFACE ( 'NONE', #2490, 2.000000000000001776 ) ;
#3283 = ADVANCED_FACE ( 'NONE', ( #796, #1329 ), #1315, .F. ) ;
#3284 = LINE ( 'NONE', #941, #1253 ) ;
#3285 = CARTESIAN_POINT ( 'NONE',  ( -44.99999999999999289, 45.00000000000000711, 10.00000000000000533 ) ) ;
#3286 = EDGE_LOOP ( 'NONE', ( #3082, #2756, #828, #2955 ) ) ;
#3287 = CARTESIAN_POINT ( 'NONE',  ( -40.00000000000000000, 136.9705627484771355, -4.999999999999995559 ) ) ;
#3288 = PRODUCT_DEFINITION_CONTEXT ( 'detailed design', #2966, 'design' ) ;
#3289 = SHAPE_DEFINITION_REPRESENTATION ( #2039, #2804 ) ;
#3290 = ORIENTED_EDGE ( 'NONE', *, *, #2774, .T. ) ;
#3291 = CARTESIAN_POINT ( 'NONE',  ( -54.99999999999995026, 120.0000000000000142, -4.999999999999997335 ) ) ;
#3292 = ADVANCED_FACE ( 'NONE', ( #2828, #1005 ), #2572, .F. ) ;
#3293 = ORIENTED_EDGE ( 'NONE', *, *, #2314, .T. ) ;
#3294 = DIRECTION ( 'NONE',  ( -1.000000000000000000, -0.000000000000000000, -0.000000000000000000 ) ) ;
#3295 = PRODUCT_DEFINITION_SHAPE ( 'NONE', 'NONE',  #3379 ) ;
#3296 = DIRECTION ( 'NONE',  ( 0.000000000000000000, -1.000000000000000000, 0.000000000000000000 ) ) ;
#3297 = DIRECTION ( 'NONE',  ( -0.000000000000000000, 1.000000000000000000, -0.000000000000000000 ) ) ;
#3298 = CARTESIAN_POINT ( 'NONE',  ( -50.00000000000000000, 52.00000000000000711, 6.000000000000004441 ) ) ;
#3299 = CARTESIAN_POINT ( 'NONE',  ( -74.99999999999998579, 50.00000000000000000, -50.00000000000000000 ) ) ;
#3300 = DIRECTION ( 'NONE',  ( -0.000000000000000000, 1.000000000000000000, -0.000000000000000000 ) ) ;
#3301 = PRODUCT_RELATED_PRODUCT_CATEGORY ( 'part', '', ( #455 ) ) ;
#3302 = EDGE_LOOP ( 'NONE', ( #1303, #354, #1423 ) ) ;
#3303 = PLANE ( 'NONE',  #1353 ) ;
#3304 = CARTESIAN_POINT ( 'NONE',  ( -44.99999999999999289, 56.00000000000000711, 10.00000000000000533 ) ) ;
#3305 = EDGE_LOOP ( 'NONE', ( #1176, #1608 ) ) ;
#3306 = FACE_OUTER_BOUND ( 'NONE', #964, .T. ) ;
#3307 = SHAPE_REPRESENTATION_RELATIONSHIP ( 'NONE' , 'NONE' ,  #714, #315 ) ;
#3308 = ORIENTED_EDGE ( 'NONE', *, *, #3237, .F. ) ;
#3309 = DIRECTION ( 'NONE',  ( 0.000000000000000000, -1.000000000000000000, 0.000000000000000000 ) ) ;
#3310 = DIRECTION ( 'NONE',  ( 1.000000000000000000, 0.000000000000000000, 0.000000000000000000 ) ) ;
#3311 = EDGE_CURVE ( 'NONE', #1531, #361, #493, .T. ) ;
#3312 = CARTESIAN_POINT ( 'NONE',  ( -40.00000000000000000, 52.00000000000000711, -14.99999999999999645 ) ) ;
#3313 = CARTESIAN_POINT ( 'NONE',  ( -66.99999999999997158, -6.000000000000000000, 41.99999999999999289 ) ) ;
#3314 = FACE_OUTER_BOUND ( 'NONE', #1016, .T. ) ;
#3315 = ADVANCED_FACE ( 'NONE', ( #507 ), #270, .F. ) ;
#3316 = CARTESIAN_POINT ( 'NONE',  ( 4.000000000000000000, 0.000000000000000000, 0.000000000000000000 ) ) ;
#3317 = COLOUR_RGB ( '',0.8941176470588234615, 0.8941176470588234615, 0.8941176470588234615 ) ;
#3318 = AXIS2_PLACEMENT_3D ( 'NONE', #937, #883, #660 ) ;
#3319 = ORIENTED_EDGE ( 'NONE', *, *, #496, .T. ) ;
#3320 = DIRECTION ( 'NONE',  ( 0.000000000000000000, 0.000000000000000000, 1.000000000000000000 ) ) ;
#3321 = APPLICATION_CONTEXT ( 'automotive_design' ) ;
#3322 = CIRCLE ( 'NONE', #1194, 2.000000000000001776 ) ;
#3323 = AXIS2_PLACEMENT_3D ( 'NONE', #383, #346, #2922 ) ;
#3324 = ORIENTED_EDGE ( 'NONE', *, *, #2652, .F. ) ;
#3325 = AXIS2_PLACEMENT_3D ( 'NONE', #1110, #2346, #552 ) ;
#3326 = VECTOR ( 'NONE', #647, 1000.000000000000000 ) ;
#3327 = EDGE_CURVE ( 'NONE', #756, #84, #1833, .T. ) ;
#3328 = DIRECTION ( 'NONE',  ( 0.000000000000000000, -9.783878858594328898E-16, -1.000000000000000000 ) ) ;
#3329 = AXIS2_PLACEMENT_3D ( 'NONE', #1603, #2434, #1938 ) ;
#3330 = CIRCLE ( 'NONE', #55, 2.499999999999995115 ) ;
#3331 =( LENGTH_UNIT ( ) NAMED_UNIT ( * ) SI_UNIT ( .MILLI., .METRE. ) );
#3332 = ORIENTED_EDGE ( 'NONE', *, *, #842, .T. ) ;
#3333 = LINE ( 'NONE', #2789, #2224 ) ;
#3334 = SURFACE_STYLE_FILL_AREA ( #1242 ) ;
#3335 = DIRECTION ( 'NONE',  ( 1.000000000000000000, 0.000000000000000000, 0.000000000000000000 ) ) ;
#3336 = CARTESIAN_POINT ( 'NONE',  ( -54.99999999999995026, 130.0000000000000000, -4.999999999999997335 ) ) ;
#3337 = CARTESIAN_POINT ( 'NONE',  ( -54.99999999999995026, 120.0000000000000142, 5.000000000000004441 ) ) ;
#3338 =( NAMED_UNIT ( * ) PLANE_ANGLE_UNIT ( ) SI_UNIT ( $, .RADIAN. ) );
#3339 = ADVANCED_FACE ( 'NONE', ( #2095 ), #2075, .F. ) ;
#3340 = VERTEX_POINT ( 'NONE', #3126 ) ;
#3341 = ORIENTED_EDGE ( 'NONE', *, *, #2868, .F. ) ;
#3342 = DIRECTION ( 'NONE',  ( -0.000000000000000000, 1.000000000000000000, -0.000000000000000000 ) ) ;
#3343 = ORIENTED_EDGE ( 'NONE', *, *, #1211, .T. ) ;
#3344 = CARTESIAN_POINT ( 'NONE',  ( -66.99999999999997158, -8.000000000000000000, 41.99999999999999289 ) ) ;
#3345 =( NAMED_UNIT ( * ) PLANE_ANGLE_UNIT ( ) SI_UNIT ( $, .RADIAN. ) );
#3346 = PRODUCT_RELATED_PRODUCT_CATEGORY ( 'part', '', ( #2796 ) ) ;
#3347 = ORIENTED_EDGE ( 'NONE', *, *, #459, .T. ) ;
#3348 = LINE ( 'NONE', #1241, #1086 ) ;
#3349 = SURFACE_STYLE_USAGE ( .BOTH. , #247 ) ;
#3350 = CARTESIAN_POINT ( 'NONE',  ( -45.00000000000000000, 52.00000000000000711, -9.999999999999994671 ) ) ;
#3351 = DIRECTION ( 'NONE',  ( 0.000000000000000000, -1.000000000000000000, 0.000000000000000000 ) ) ;
#3352 = PRODUCT_DEFINITION_SHAPE ( 'NONE', 'NONE',  #2025 ) ;
#3353 = VERTEX_POINT ( 'NONE', #1805 ) ;
#3354 = ORIENTED_EDGE ( 'NONE', *, *, #3252, .F. ) ;
#3355 = ORIENTED_EDGE ( 'NONE', *, *, #24, .T. ) ;
#3356 = DIRECTION ( 'NONE',  ( 0.000000000000000000, -0.000000000000000000, -1.000000000000000000 ) ) ;
#3357 = EDGE_CURVE ( 'NONE', #787, #1848, #2300, .T. ) ;
#3358 = ITEM_DEFINED_TRANSFORMATION ( 'NONE', 'NONE', #2566,  #3111 ) ;
#3359 = EDGE_LOOP ( 'NONE', ( #2155, #176, #307, #1374 ) ) ;
#3360 = DIRECTION ( 'NONE',  ( 0.000000000000000000, -1.000000000000000000, 0.000000000000000000 ) ) ;
#3361 = EDGE_LOOP ( 'NONE', ( #1035, #576, #3075 ) ) ;
#3362 = DIRECTION ( 'NONE',  ( 0.000000000000000000, -1.000000000000000000, 0.000000000000000000 ) ) ;
#3363 = CARTESIAN_POINT ( 'NONE',  ( 0.000000000000000000, 25.00000000000000000, 47.00000000000000000 ) ) ;
#3364 = CARTESIAN_POINT ( 'NONE',  ( -66.99999999999997158, 0.000000000000000000, 41.99999999999999289 ) ) ;
#3365 = CARTESIAN_POINT ( 'NONE',  ( 2.000000000000000000, 0.000000000000000000, 0.000000000000000000 ) ) ;
#3366 = CARTESIAN_POINT ( 'NONE',  ( -49.99999999999999289, 52.00000000000000711, 5.000000000000007994 ) ) ;
#3367 = CLOSED_SHELL ( 'NONE', ( #2759, #2569, #855, #177, #1144, #1444, #2122, #1063, #1261, #2974, #1271, #3283, #983, #3098 ) ) ;
#3368 = CARTESIAN_POINT ( 'NONE',  ( 55.00000000000004974, 130.0000000000000000, 5.000000000000004441 ) ) ;
#3369 = ORIENTED_EDGE ( 'NONE', *, *, #467, .T. ) ;
#3370 = ORIENTED_EDGE ( 'NONE', *, *, #3273, .F. ) ;
#3371 = CARTESIAN_POINT ( 'NONE',  ( -54.99999999999995026, 130.0000000000000000, 5.000000000000004441 ) ) ;
#3372 = DIRECTION ( 'NONE',  ( 1.000000000000000000, 0.000000000000000000, -0.000000000000000000 ) ) ;
#3373 = NEXT_ASSEMBLY_USAGE_OCCURRENCE ( 'NAUO1', ' ', ' ', #2270, #66, $ ) ;
#3374 = NEXT_ASSEMBLY_USAGE_OCCURRENCE ( 'NAUO2', ' ', ' ', #2270, #2584, $ ) ;
#3375 = NEXT_ASSEMBLY_USAGE_OCCURRENCE ( 'NAUO3', ' ', ' ', #2270, #2980, $ ) ;
#3376 = NEXT_ASSEMBLY_USAGE_OCCURRENCE ( 'NAUO4', ' ', ' ', #2270, #2025, $ ) ;
#3377 = NEXT_ASSEMBLY_USAGE_OCCURRENCE ( 'NAUO5', ' ', ' ', #2270, #3197, $ ) ;
#3378 = NEXT_ASSEMBLY_USAGE_OCCURRENCE ( 'NAUO6', ' ', ' ', #2270, #1526, $ ) ;
#3379 = NEXT_ASSEMBLY_USAGE_OCCURRENCE ( 'NAUO7', ' ', ' ', #2270, #2584, $ ) ;
#3380 = NEXT_ASSEMBLY_USAGE_OCCURRENCE ( 'NAUO8', ' ', ' ', #2270, #2584, $ ) ;
#3381 = NEXT_ASSEMBLY_USAGE_OCCURRENCE ( 'NAUO9', ' ', ' ', #2270, #2584, $ ) ;
#3382 = NEXT_ASSEMBLY_USAGE_OCCURRENCE ( 'NAUO10', ' ', ' ', #2270, #1526, $ ) ;
#3383 = NEXT_ASSEMBLY_USAGE_OCCURRENCE ( 'NAUO11', ' ', ' ', #2270, #2980, $ ) ;
#3384 = NEXT_ASSEMBLY_USAGE_OCCURRENCE ( 'NAUO12', ' ', ' ', #2270, #273, $ ) ;
#3385 = NEXT_ASSEMBLY_USAGE_OCCURRENCE ( 'NAUO13', ' ', ' ', #2270, #273, $ ) ;
#3386 = NEXT_ASSEMBLY_USAGE_OCCURRENCE ( 'NAUO14', ' ', ' ', #2270, #273, $ ) ;
#3387 = NEXT_ASSEMBLY_USAGE_OCCURRENCE ( 'NAUO15', ' ', ' ', #2270, #273, $ ) ;
#3388=COLOUR_RGB('Dark Blue',0.08,0.2,0.34);
#3389=FILL_AREA_STYLE_COLOUR('',#3388);
#3390=FILL_AREA_STYLE('',(#3389));
#3391=SURFACE_STYLE_FILL_AREA(#3390);
#3392=SURFACE_SIDE_STYLE('',(#3391));
#3393=SURFACE_STYLE_USAGE(.BOTH.,#3392);
#3394=PRESENTATION_STYLE_ASSIGNMENT((#3393));
#3395=COLOUR_RGB('Light Blue',0.38,0.62,0.78);
#3396=FILL_AREA_STYLE_COLOUR('',#3395);
#3397=FILL_AREA_STYLE('',(#3396));
#3398=SURFACE_STYLE_FILL_AREA(#3397);
#3399=SURFACE_SIDE_STYLE('',(#3398));
#3400=SURFACE_STYLE_USAGE(.BOTH.,#3399);
#3401=PRESENTATION_STYLE_ASSIGNMENT((#3400));
#3402=COLOUR_RGB('Sky Blue',0.24,0.69,0.87);
#3403=FILL_AREA_STYLE_COLOUR('',#3402);
#3404=FILL_AREA_STYLE('',(#3403));
#3405=SURFACE_STYLE_FILL_AREA(#3404);
#3406=SURFACE_SIDE_STYLE('',(#3405));
#3407=SURFACE_STYLE_USAGE(.BOTH.,#3406);
#3408=PRESENTATION_STYLE_ASSIGNMENT((#3407));
#3409=COLOUR_RGB('Grey',0.48,0.52,0.57);
#3410=FILL_AREA_STYLE_COLOUR('',#3409);
#3411=FILL_AREA_STYLE('',(#3410));
#3412=SURFACE_STYLE_FILL_AREA(#3411);
#3413=SURFACE_SIDE_STYLE('',(#3412));
#3414=SURFACE_STYLE_USAGE(.BOTH.,#3413);
#3415=PRESENTATION_STYLE_ASSIGNMENT((#3414));
#3416=COLOUR_RGB('Black',0.12,0.14,0.17);
#3417=FILL_AREA_STYLE_COLOUR('',#3416);
#3418=FILL_AREA_STYLE('',(#3417));
#3419=SURFACE_STYLE_FILL_AREA(#3418);
#3420=SURFACE_SIDE_STYLE('',(#3419));
#3421=SURFACE_STYLE_USAGE(.BOTH.,#3420);
#3422=PRESENTATION_STYLE_ASSIGNMENT((#3421));
#3423=COLOUR_RGB('Off White',0.89,0.88,0.83);
#3424=FILL_AREA_STYLE_COLOUR('',#3423);
#3425=FILL_AREA_STYLE('',(#3424));
#3426=SURFACE_STYLE_FILL_AREA(#3425);
#3427=SURFACE_SIDE_STYLE('',(#3426));
#3428=SURFACE_STYLE_USAGE(.BOTH.,#3427);
#3429=PRESENTATION_STYLE_ASSIGNMENT((#3428));
ENDSEC;
END-ISO-10303-21;
